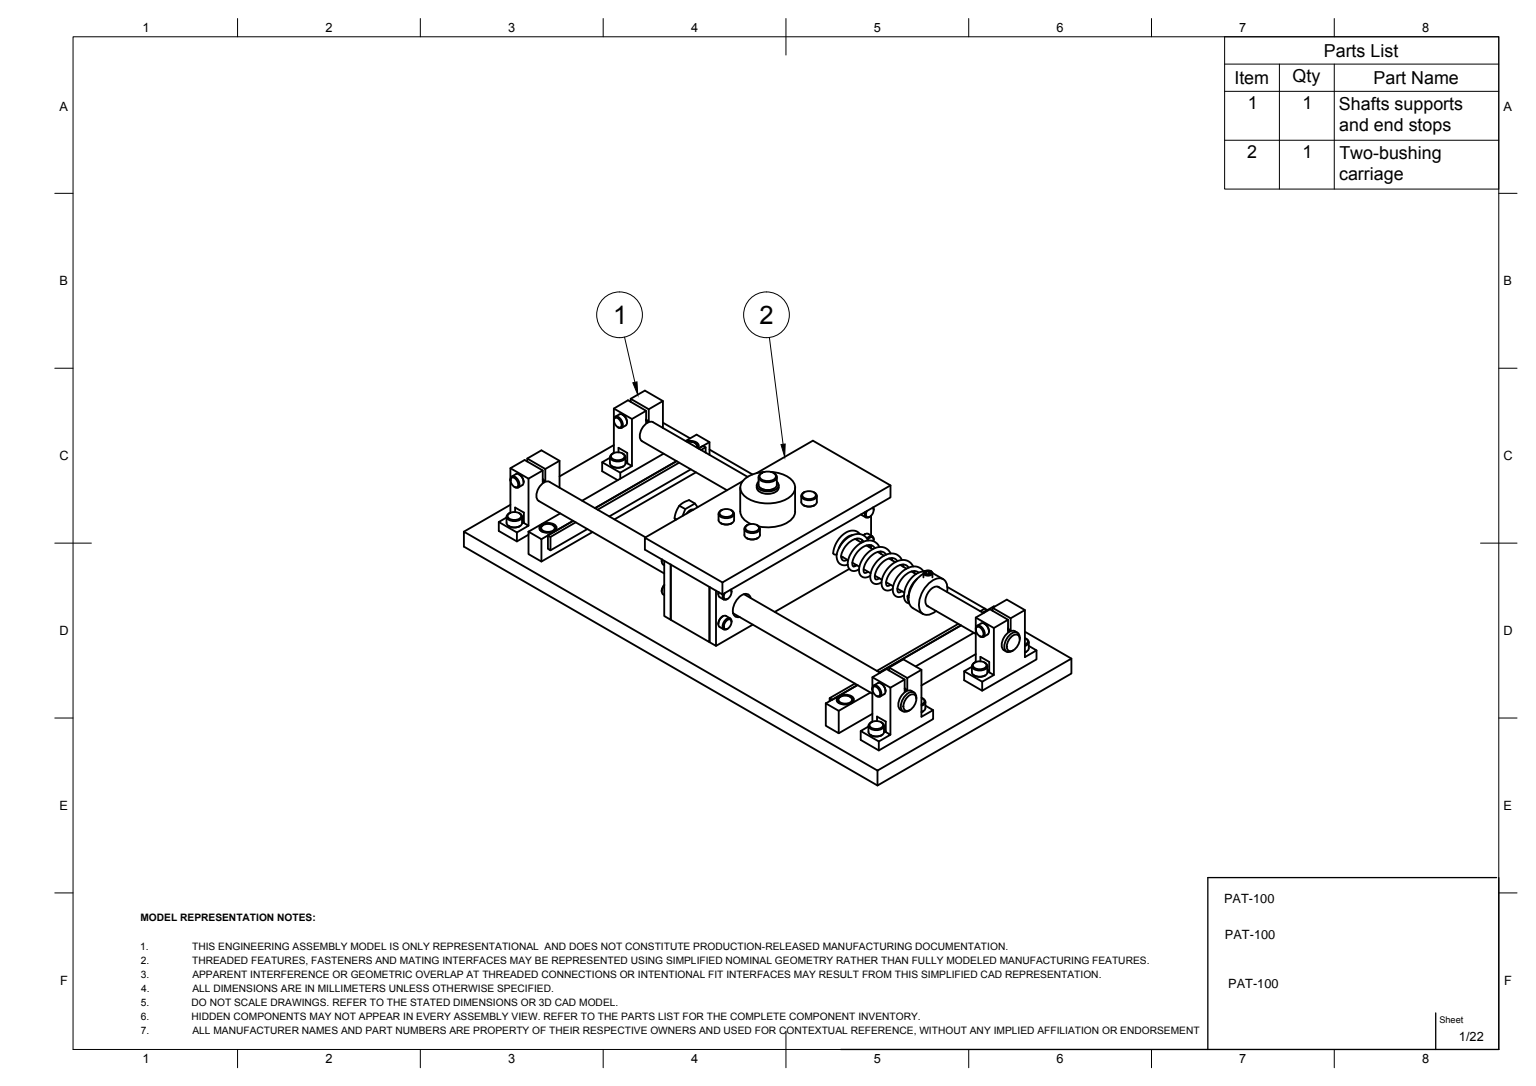
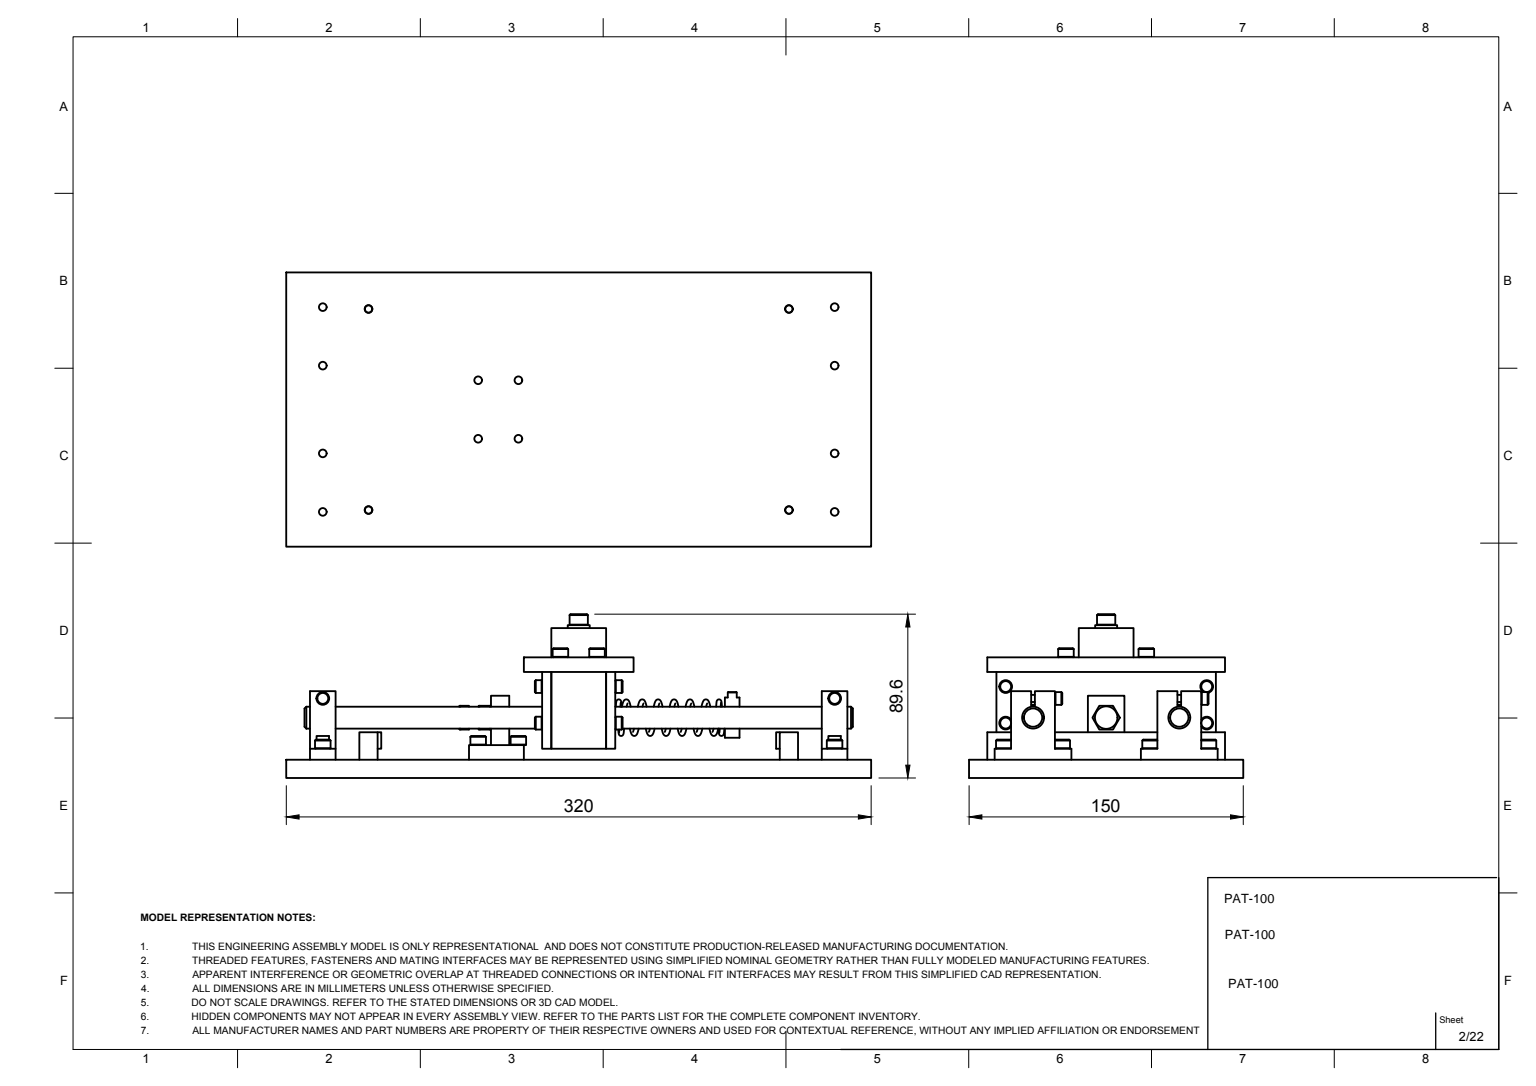
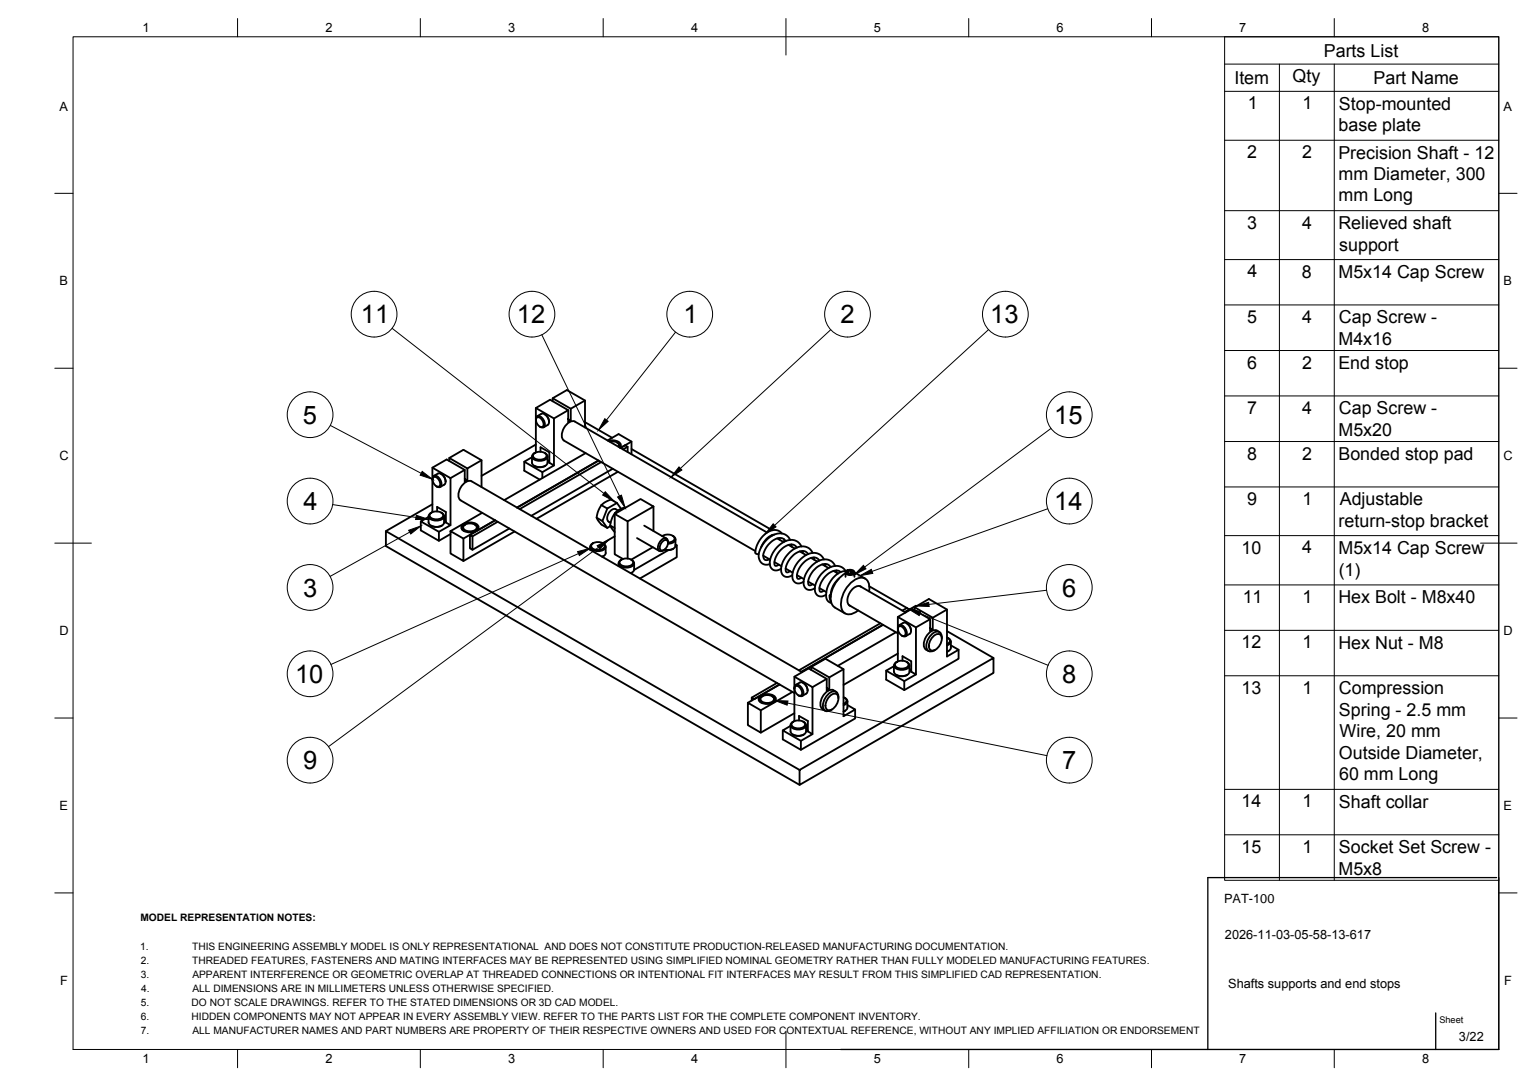
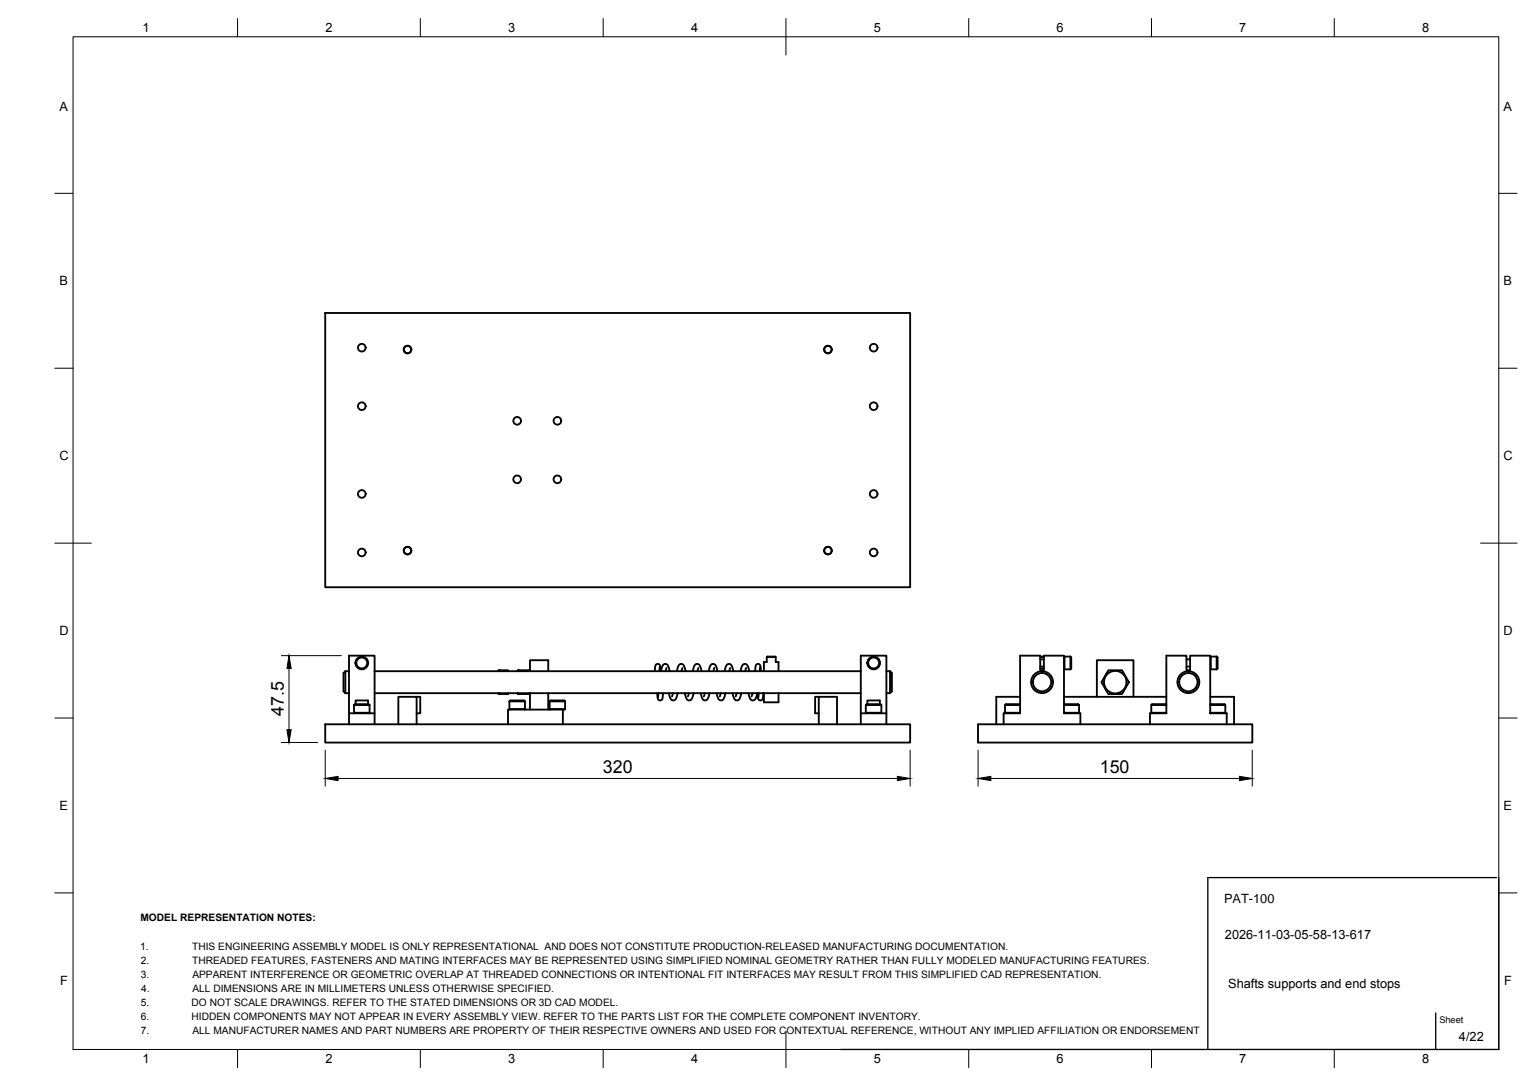
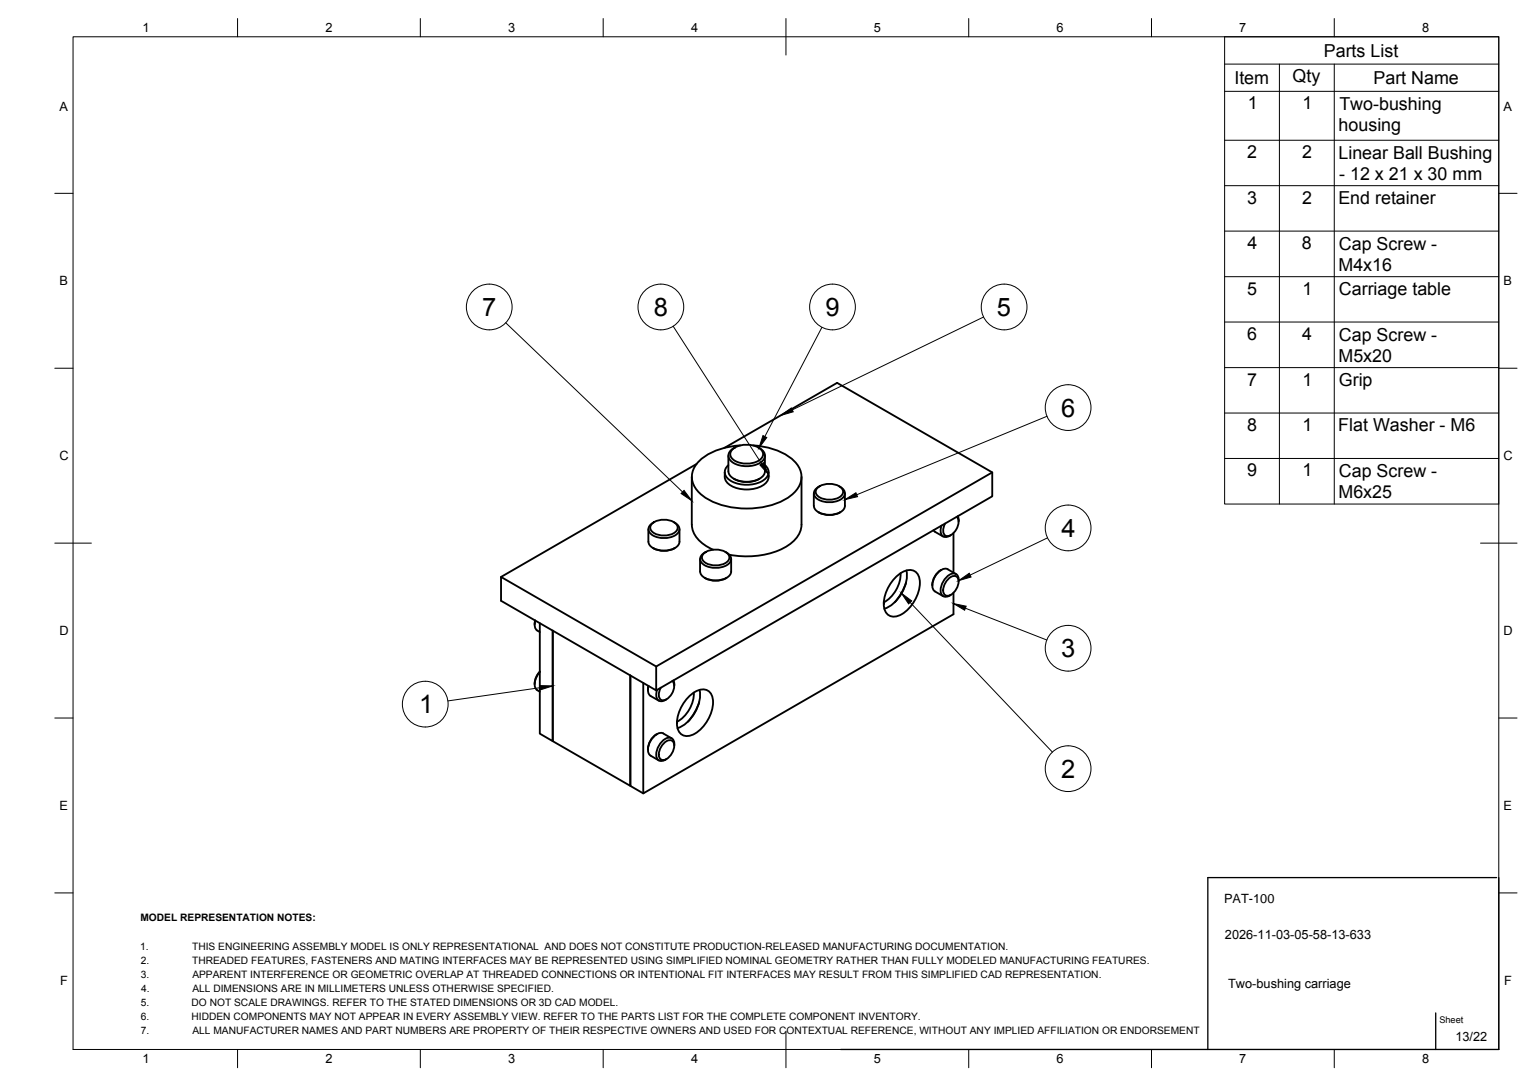
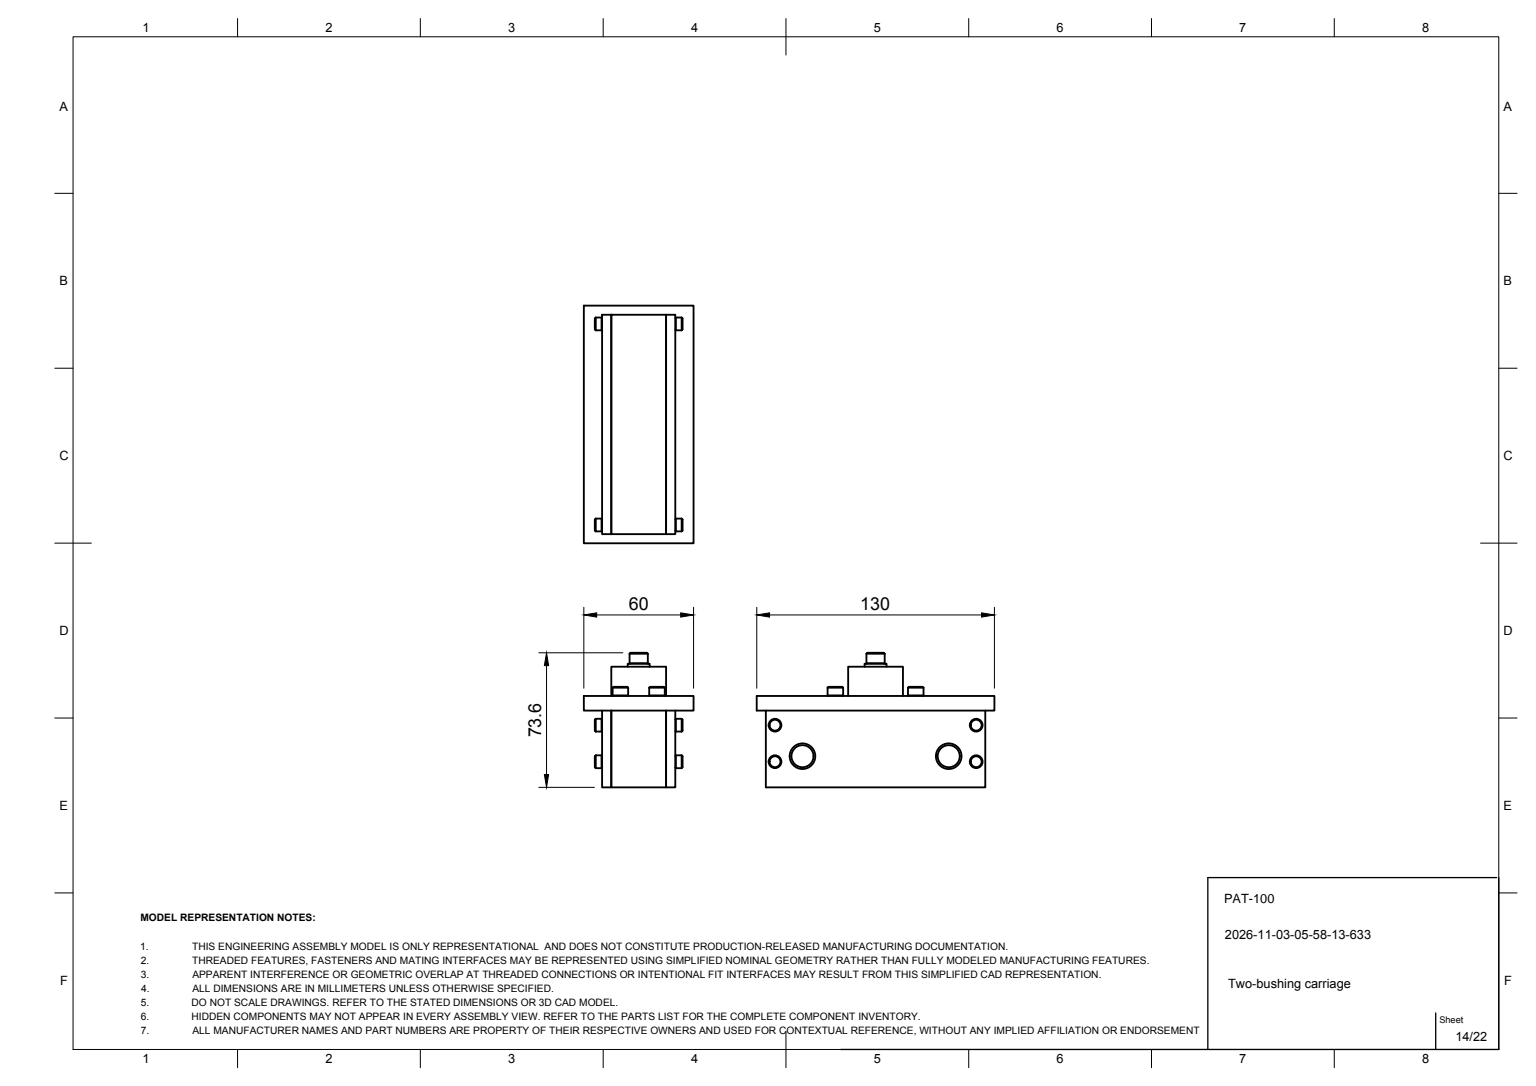
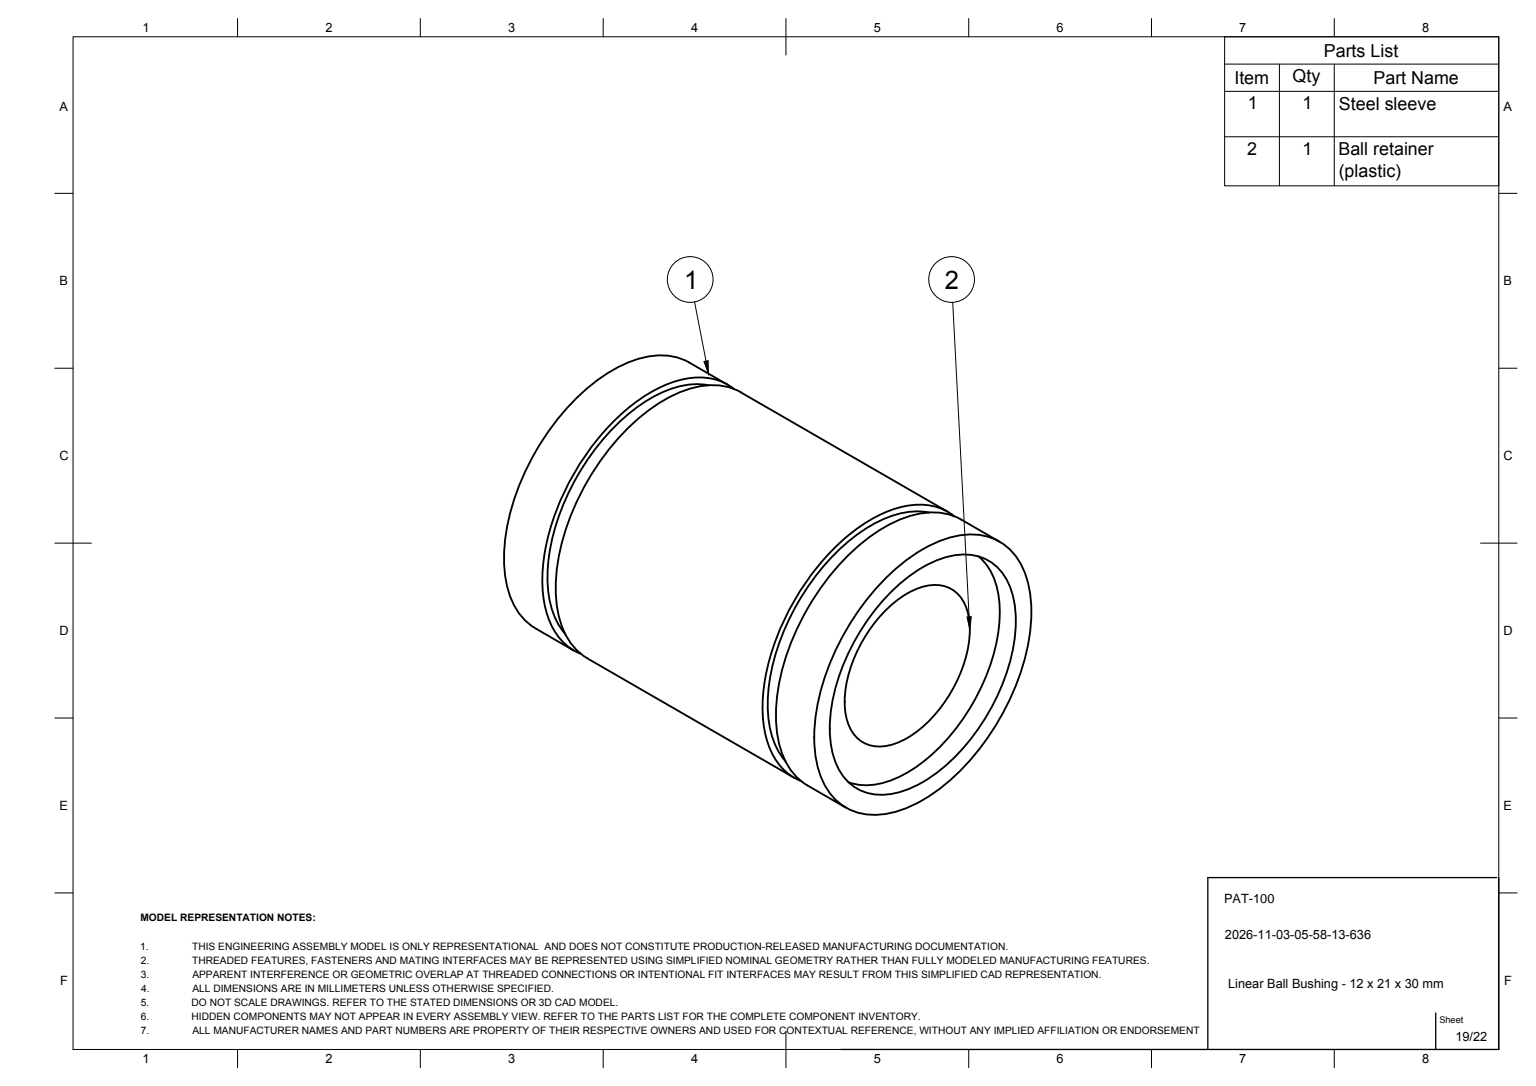
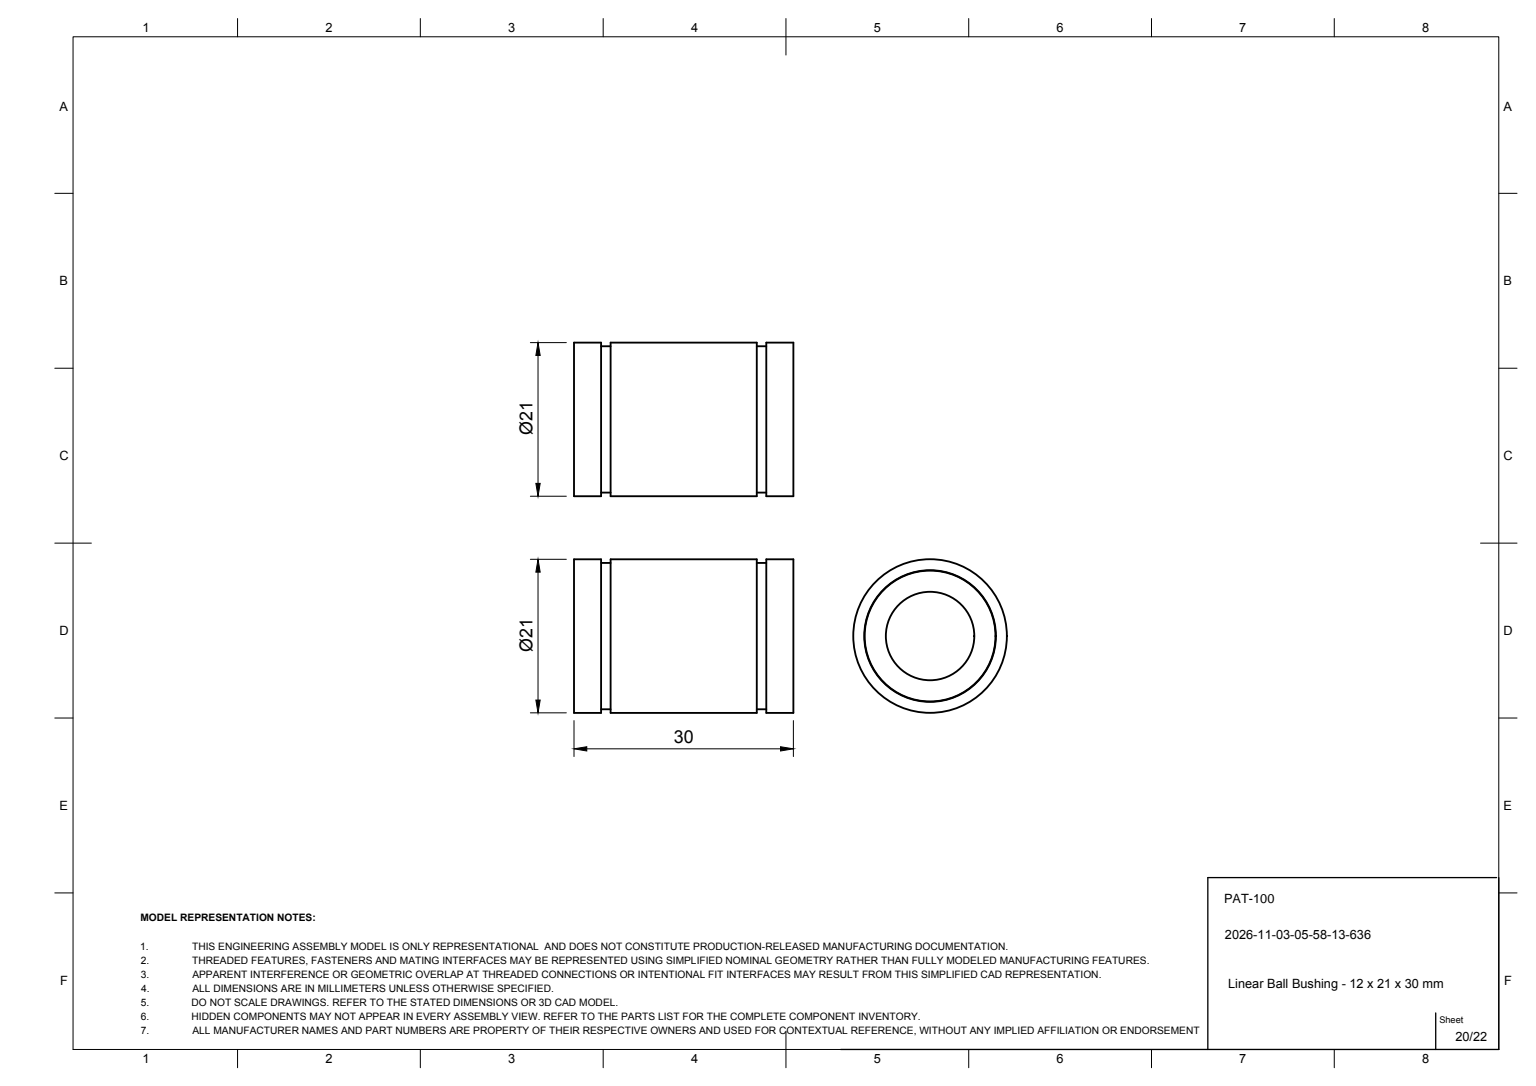
ISO-10303-21;
HEADER;
/* Generated by software containing ST-Developer
 * from STEP Tools, Inc. (www.steptools.com) 
 */

FILE_DESCRIPTION(
/* description */ (''),
/* implementation_level */ '2;1');

FILE_NAME(
/* name */ 'PAT-100',
/* time_stamp */ '2026-10-29T16:43:51-07:00',
/* author */ (''),
/* organization */ (''),
/* preprocessor_version */ 'ST-DEVELOPER v20.2',
/* originating_system */ 'Autodesk Translation Framework v15.17.0.0',
/* authorisation */ '');

FILE_SCHEMA (('AUTOMOTIVE_DESIGN { 1 0 10303 214 3 1 1 }'));
ENDSEC;

DATA;
#10=MECHANICAL_DESIGN_GEOMETRIC_PRESENTATION_REPRESENTATION('',(#365,#366,
#367,#368,#369,#370,#371,#372,#373,#374,#375,#376,#377,#378,#379,#380,#381,
#382,#383,#384,#385,#386,#387),#10292);
#11=ITEM_DEFINED_TRANSFORMATION($,$,#5632,#5681);
#12=ITEM_DEFINED_TRANSFORMATION($,$,#5664,#5682);
#13=ITEM_DEFINED_TRANSFORMATION($,$,#5291,#5760);
#14=ITEM_DEFINED_TRANSFORMATION($,$,#5346,#5761);
#15=ITEM_DEFINED_TRANSFORMATION($,$,#5356,#5762);
#16=ITEM_DEFINED_TRANSFORMATION($,$,#5394,#5763);
#17=ITEM_DEFINED_TRANSFORMATION($,$,#5394,#5764);
#18=ITEM_DEFINED_TRANSFORMATION($,$,#5708,#5765);
#19=ITEM_DEFINED_TRANSFORMATION($,$,#5356,#5766);
#20=ITEM_DEFINED_TRANSFORMATION($,$,#5394,#5767);
#21=ITEM_DEFINED_TRANSFORMATION($,$,#5394,#5768);
#22=ITEM_DEFINED_TRANSFORMATION($,$,#5708,#5769);
#23=ITEM_DEFINED_TRANSFORMATION($,$,#5346,#5770);
#24=ITEM_DEFINED_TRANSFORMATION($,$,#5356,#5771);
#25=ITEM_DEFINED_TRANSFORMATION($,$,#5394,#5772);
#26=ITEM_DEFINED_TRANSFORMATION($,$,#5394,#5773);
#27=ITEM_DEFINED_TRANSFORMATION($,$,#5708,#5774);
#28=ITEM_DEFINED_TRANSFORMATION($,$,#5356,#5775);
#29=ITEM_DEFINED_TRANSFORMATION($,$,#5394,#5776);
#30=ITEM_DEFINED_TRANSFORMATION($,$,#5394,#5777);
#31=ITEM_DEFINED_TRANSFORMATION($,$,#5708,#5778);
#32=ITEM_DEFINED_TRANSFORMATION($,$,#5418,#5779);
#33=ITEM_DEFINED_TRANSFORMATION($,$,#5734,#5780);
#34=ITEM_DEFINED_TRANSFORMATION($,$,#5734,#5781);
#35=ITEM_DEFINED_TRANSFORMATION($,$,#5418,#5782);
#36=ITEM_DEFINED_TRANSFORMATION($,$,#5734,#5783);
#37=ITEM_DEFINED_TRANSFORMATION($,$,#5734,#5784);
#38=ITEM_DEFINED_TRANSFORMATION($,$,#5439,#5785);
#39=ITEM_DEFINED_TRANSFORMATION($,$,#5439,#5786);
#40=ITEM_DEFINED_TRANSFORMATION($,$,#5446,#5787);
#41=ITEM_DEFINED_TRANSFORMATION($,$,#5473,#5788);
#42=ITEM_DEFINED_TRANSFORMATION($,$,#5473,#5789);
#43=ITEM_DEFINED_TRANSFORMATION($,$,#5473,#5790);
#44=ITEM_DEFINED_TRANSFORMATION($,$,#5473,#5791);
#45=ITEM_DEFINED_TRANSFORMATION($,$,#5497,#5792);
#46=ITEM_DEFINED_TRANSFORMATION($,$,#5514,#5793);
#47=ITEM_DEFINED_TRANSFORMATION($,$,#5530,#5794);
#48=ITEM_DEFINED_TRANSFORMATION($,$,#5535,#5795);
#49=ITEM_DEFINED_TRANSFORMATION($,$,#5550,#5796);
#50=ITEM_DEFINED_TRANSFORMATION($,$,#5568,#5841);
#51=ITEM_DEFINED_TRANSFORMATION($,$,#5609,#5842);
#52=ITEM_DEFINED_TRANSFORMATION($,$,#5631,#5843);
#53=ITEM_DEFINED_TRANSFORMATION($,$,#5631,#5844);
#54=ITEM_DEFINED_TRANSFORMATION($,$,#5683,#5845);
#55=ITEM_DEFINED_TRANSFORMATION($,$,#5683,#5846);
#56=ITEM_DEFINED_TRANSFORMATION($,$,#5708,#5847);
#57=ITEM_DEFINED_TRANSFORMATION($,$,#5708,#5848);
#58=ITEM_DEFINED_TRANSFORMATION($,$,#5708,#5849);
#59=ITEM_DEFINED_TRANSFORMATION($,$,#5708,#5850);
#60=ITEM_DEFINED_TRANSFORMATION($,$,#5708,#5851);
#61=ITEM_DEFINED_TRANSFORMATION($,$,#5708,#5852);
#62=ITEM_DEFINED_TRANSFORMATION($,$,#5708,#5853);
#63=ITEM_DEFINED_TRANSFORMATION($,$,#5708,#5854);
#64=ITEM_DEFINED_TRANSFORMATION($,$,#5734,#5855);
#65=ITEM_DEFINED_TRANSFORMATION($,$,#5734,#5856);
#66=ITEM_DEFINED_TRANSFORMATION($,$,#5734,#5857);
#67=ITEM_DEFINED_TRANSFORMATION($,$,#5734,#5858);
#68=ITEM_DEFINED_TRANSFORMATION($,$,#5797,#5859);
#69=ITEM_DEFINED_TRANSFORMATION($,$,#5806,#5860);
#70=ITEM_DEFINED_TRANSFORMATION($,$,#5815,#5861);
#71=ITEM_DEFINED_TRANSFORMATION($,$,#5290,#5862);
#72=ITEM_DEFINED_TRANSFORMATION($,$,#5567,#5863);
#73=(
REPRESENTATION_RELATIONSHIP($,$,#10432,#10431)
REPRESENTATION_RELATIONSHIP_WITH_TRANSFORMATION(#11)
SHAPE_REPRESENTATION_RELATIONSHIP()
);
#74=(
REPRESENTATION_RELATIONSHIP($,$,#10433,#10431)
REPRESENTATION_RELATIONSHIP_WITH_TRANSFORMATION(#12)
SHAPE_REPRESENTATION_RELATIONSHIP()
);
#75=(
REPRESENTATION_RELATIONSHIP($,$,#10415,#10414)
REPRESENTATION_RELATIONSHIP_WITH_TRANSFORMATION(#13)
SHAPE_REPRESENTATION_RELATIONSHIP()
);
#76=(
REPRESENTATION_RELATIONSHIP($,$,#10416,#10414)
REPRESENTATION_RELATIONSHIP_WITH_TRANSFORMATION(#14)
SHAPE_REPRESENTATION_RELATIONSHIP()
);
#77=(
REPRESENTATION_RELATIONSHIP($,$,#10417,#10414)
REPRESENTATION_RELATIONSHIP_WITH_TRANSFORMATION(#15)
SHAPE_REPRESENTATION_RELATIONSHIP()
);
#78=(
REPRESENTATION_RELATIONSHIP($,$,#10418,#10414)
REPRESENTATION_RELATIONSHIP_WITH_TRANSFORMATION(#16)
SHAPE_REPRESENTATION_RELATIONSHIP()
);
#79=(
REPRESENTATION_RELATIONSHIP($,$,#10418,#10414)
REPRESENTATION_RELATIONSHIP_WITH_TRANSFORMATION(#17)
SHAPE_REPRESENTATION_RELATIONSHIP()
);
#80=(
REPRESENTATION_RELATIONSHIP($,$,#10435,#10414)
REPRESENTATION_RELATIONSHIP_WITH_TRANSFORMATION(#18)
SHAPE_REPRESENTATION_RELATIONSHIP()
);
#81=(
REPRESENTATION_RELATIONSHIP($,$,#10417,#10414)
REPRESENTATION_RELATIONSHIP_WITH_TRANSFORMATION(#19)
SHAPE_REPRESENTATION_RELATIONSHIP()
);
#82=(
REPRESENTATION_RELATIONSHIP($,$,#10418,#10414)
REPRESENTATION_RELATIONSHIP_WITH_TRANSFORMATION(#20)
SHAPE_REPRESENTATION_RELATIONSHIP()
);
#83=(
REPRESENTATION_RELATIONSHIP($,$,#10418,#10414)
REPRESENTATION_RELATIONSHIP_WITH_TRANSFORMATION(#21)
SHAPE_REPRESENTATION_RELATIONSHIP()
);
#84=(
REPRESENTATION_RELATIONSHIP($,$,#10435,#10414)
REPRESENTATION_RELATIONSHIP_WITH_TRANSFORMATION(#22)
SHAPE_REPRESENTATION_RELATIONSHIP()
);
#85=(
REPRESENTATION_RELATIONSHIP($,$,#10416,#10414)
REPRESENTATION_RELATIONSHIP_WITH_TRANSFORMATION(#23)
SHAPE_REPRESENTATION_RELATIONSHIP()
);
#86=(
REPRESENTATION_RELATIONSHIP($,$,#10417,#10414)
REPRESENTATION_RELATIONSHIP_WITH_TRANSFORMATION(#24)
SHAPE_REPRESENTATION_RELATIONSHIP()
);
#87=(
REPRESENTATION_RELATIONSHIP($,$,#10418,#10414)
REPRESENTATION_RELATIONSHIP_WITH_TRANSFORMATION(#25)
SHAPE_REPRESENTATION_RELATIONSHIP()
);
#88=(
REPRESENTATION_RELATIONSHIP($,$,#10418,#10414)
REPRESENTATION_RELATIONSHIP_WITH_TRANSFORMATION(#26)
SHAPE_REPRESENTATION_RELATIONSHIP()
);
#89=(
REPRESENTATION_RELATIONSHIP($,$,#10435,#10414)
REPRESENTATION_RELATIONSHIP_WITH_TRANSFORMATION(#27)
SHAPE_REPRESENTATION_RELATIONSHIP()
);
#90=(
REPRESENTATION_RELATIONSHIP($,$,#10417,#10414)
REPRESENTATION_RELATIONSHIP_WITH_TRANSFORMATION(#28)
SHAPE_REPRESENTATION_RELATIONSHIP()
);
#91=(
REPRESENTATION_RELATIONSHIP($,$,#10418,#10414)
REPRESENTATION_RELATIONSHIP_WITH_TRANSFORMATION(#29)
SHAPE_REPRESENTATION_RELATIONSHIP()
);
#92=(
REPRESENTATION_RELATIONSHIP($,$,#10418,#10414)
REPRESENTATION_RELATIONSHIP_WITH_TRANSFORMATION(#30)
SHAPE_REPRESENTATION_RELATIONSHIP()
);
#93=(
REPRESENTATION_RELATIONSHIP($,$,#10435,#10414)
REPRESENTATION_RELATIONSHIP_WITH_TRANSFORMATION(#31)
SHAPE_REPRESENTATION_RELATIONSHIP()
);
#94=(
REPRESENTATION_RELATIONSHIP($,$,#10419,#10414)
REPRESENTATION_RELATIONSHIP_WITH_TRANSFORMATION(#32)
SHAPE_REPRESENTATION_RELATIONSHIP()
);
#95=(
REPRESENTATION_RELATIONSHIP($,$,#10436,#10414)
REPRESENTATION_RELATIONSHIP_WITH_TRANSFORMATION(#33)
SHAPE_REPRESENTATION_RELATIONSHIP()
);
#96=(
REPRESENTATION_RELATIONSHIP($,$,#10436,#10414)
REPRESENTATION_RELATIONSHIP_WITH_TRANSFORMATION(#34)
SHAPE_REPRESENTATION_RELATIONSHIP()
);
#97=(
REPRESENTATION_RELATIONSHIP($,$,#10419,#10414)
REPRESENTATION_RELATIONSHIP_WITH_TRANSFORMATION(#35)
SHAPE_REPRESENTATION_RELATIONSHIP()
);
#98=(
REPRESENTATION_RELATIONSHIP($,$,#10436,#10414)
REPRESENTATION_RELATIONSHIP_WITH_TRANSFORMATION(#36)
SHAPE_REPRESENTATION_RELATIONSHIP()
);
#99=(
REPRESENTATION_RELATIONSHIP($,$,#10436,#10414)
REPRESENTATION_RELATIONSHIP_WITH_TRANSFORMATION(#37)
SHAPE_REPRESENTATION_RELATIONSHIP()
);
#100=(
REPRESENTATION_RELATIONSHIP($,$,#10420,#10414)
REPRESENTATION_RELATIONSHIP_WITH_TRANSFORMATION(#38)
SHAPE_REPRESENTATION_RELATIONSHIP()
);
#101=(
REPRESENTATION_RELATIONSHIP($,$,#10420,#10414)
REPRESENTATION_RELATIONSHIP_WITH_TRANSFORMATION(#39)
SHAPE_REPRESENTATION_RELATIONSHIP()
);
#102=(
REPRESENTATION_RELATIONSHIP($,$,#10421,#10414)
REPRESENTATION_RELATIONSHIP_WITH_TRANSFORMATION(#40)
SHAPE_REPRESENTATION_RELATIONSHIP()
);
#103=(
REPRESENTATION_RELATIONSHIP($,$,#10422,#10414)
REPRESENTATION_RELATIONSHIP_WITH_TRANSFORMATION(#41)
SHAPE_REPRESENTATION_RELATIONSHIP()
);
#104=(
REPRESENTATION_RELATIONSHIP($,$,#10422,#10414)
REPRESENTATION_RELATIONSHIP_WITH_TRANSFORMATION(#42)
SHAPE_REPRESENTATION_RELATIONSHIP()
);
#105=(
REPRESENTATION_RELATIONSHIP($,$,#10422,#10414)
REPRESENTATION_RELATIONSHIP_WITH_TRANSFORMATION(#43)
SHAPE_REPRESENTATION_RELATIONSHIP()
);
#106=(
REPRESENTATION_RELATIONSHIP($,$,#10422,#10414)
REPRESENTATION_RELATIONSHIP_WITH_TRANSFORMATION(#44)
SHAPE_REPRESENTATION_RELATIONSHIP()
);
#107=(
REPRESENTATION_RELATIONSHIP($,$,#10423,#10414)
REPRESENTATION_RELATIONSHIP_WITH_TRANSFORMATION(#45)
SHAPE_REPRESENTATION_RELATIONSHIP()
);
#108=(
REPRESENTATION_RELATIONSHIP($,$,#10424,#10414)
REPRESENTATION_RELATIONSHIP_WITH_TRANSFORMATION(#46)
SHAPE_REPRESENTATION_RELATIONSHIP()
);
#109=(
REPRESENTATION_RELATIONSHIP($,$,#10425,#10414)
REPRESENTATION_RELATIONSHIP_WITH_TRANSFORMATION(#47)
SHAPE_REPRESENTATION_RELATIONSHIP()
);
#110=(
REPRESENTATION_RELATIONSHIP($,$,#10426,#10414)
REPRESENTATION_RELATIONSHIP_WITH_TRANSFORMATION(#48)
SHAPE_REPRESENTATION_RELATIONSHIP()
);
#111=(
REPRESENTATION_RELATIONSHIP($,$,#10427,#10414)
REPRESENTATION_RELATIONSHIP_WITH_TRANSFORMATION(#49)
SHAPE_REPRESENTATION_RELATIONSHIP()
);
#112=(
REPRESENTATION_RELATIONSHIP($,$,#10429,#10428)
REPRESENTATION_RELATIONSHIP_WITH_TRANSFORMATION(#50)
SHAPE_REPRESENTATION_RELATIONSHIP()
);
#113=(
REPRESENTATION_RELATIONSHIP($,$,#10430,#10428)
REPRESENTATION_RELATIONSHIP_WITH_TRANSFORMATION(#51)
SHAPE_REPRESENTATION_RELATIONSHIP()
);
#114=(
REPRESENTATION_RELATIONSHIP($,$,#10431,#10428)
REPRESENTATION_RELATIONSHIP_WITH_TRANSFORMATION(#52)
SHAPE_REPRESENTATION_RELATIONSHIP()
);
#115=(
REPRESENTATION_RELATIONSHIP($,$,#10431,#10428)
REPRESENTATION_RELATIONSHIP_WITH_TRANSFORMATION(#53)
SHAPE_REPRESENTATION_RELATIONSHIP()
);
#116=(
REPRESENTATION_RELATIONSHIP($,$,#10434,#10428)
REPRESENTATION_RELATIONSHIP_WITH_TRANSFORMATION(#54)
SHAPE_REPRESENTATION_RELATIONSHIP()
);
#117=(
REPRESENTATION_RELATIONSHIP($,$,#10434,#10428)
REPRESENTATION_RELATIONSHIP_WITH_TRANSFORMATION(#55)
SHAPE_REPRESENTATION_RELATIONSHIP()
);
#118=(
REPRESENTATION_RELATIONSHIP($,$,#10435,#10428)
REPRESENTATION_RELATIONSHIP_WITH_TRANSFORMATION(#56)
SHAPE_REPRESENTATION_RELATIONSHIP()
);
#119=(
REPRESENTATION_RELATIONSHIP($,$,#10435,#10428)
REPRESENTATION_RELATIONSHIP_WITH_TRANSFORMATION(#57)
SHAPE_REPRESENTATION_RELATIONSHIP()
);
#120=(
REPRESENTATION_RELATIONSHIP($,$,#10435,#10428)
REPRESENTATION_RELATIONSHIP_WITH_TRANSFORMATION(#58)
SHAPE_REPRESENTATION_RELATIONSHIP()
);
#121=(
REPRESENTATION_RELATIONSHIP($,$,#10435,#10428)
REPRESENTATION_RELATIONSHIP_WITH_TRANSFORMATION(#59)
SHAPE_REPRESENTATION_RELATIONSHIP()
);
#122=(
REPRESENTATION_RELATIONSHIP($,$,#10435,#10428)
REPRESENTATION_RELATIONSHIP_WITH_TRANSFORMATION(#60)
SHAPE_REPRESENTATION_RELATIONSHIP()
);
#123=(
REPRESENTATION_RELATIONSHIP($,$,#10435,#10428)
REPRESENTATION_RELATIONSHIP_WITH_TRANSFORMATION(#61)
SHAPE_REPRESENTATION_RELATIONSHIP()
);
#124=(
REPRESENTATION_RELATIONSHIP($,$,#10435,#10428)
REPRESENTATION_RELATIONSHIP_WITH_TRANSFORMATION(#62)
SHAPE_REPRESENTATION_RELATIONSHIP()
);
#125=(
REPRESENTATION_RELATIONSHIP($,$,#10435,#10428)
REPRESENTATION_RELATIONSHIP_WITH_TRANSFORMATION(#63)
SHAPE_REPRESENTATION_RELATIONSHIP()
);
#126=(
REPRESENTATION_RELATIONSHIP($,$,#10436,#10428)
REPRESENTATION_RELATIONSHIP_WITH_TRANSFORMATION(#64)
SHAPE_REPRESENTATION_RELATIONSHIP()
);
#127=(
REPRESENTATION_RELATIONSHIP($,$,#10436,#10428)
REPRESENTATION_RELATIONSHIP_WITH_TRANSFORMATION(#65)
SHAPE_REPRESENTATION_RELATIONSHIP()
);
#128=(
REPRESENTATION_RELATIONSHIP($,$,#10436,#10428)
REPRESENTATION_RELATIONSHIP_WITH_TRANSFORMATION(#66)
SHAPE_REPRESENTATION_RELATIONSHIP()
);
#129=(
REPRESENTATION_RELATIONSHIP($,$,#10436,#10428)
REPRESENTATION_RELATIONSHIP_WITH_TRANSFORMATION(#67)
SHAPE_REPRESENTATION_RELATIONSHIP()
);
#130=(
REPRESENTATION_RELATIONSHIP($,$,#10437,#10428)
REPRESENTATION_RELATIONSHIP_WITH_TRANSFORMATION(#68)
SHAPE_REPRESENTATION_RELATIONSHIP()
);
#131=(
REPRESENTATION_RELATIONSHIP($,$,#10438,#10428)
REPRESENTATION_RELATIONSHIP_WITH_TRANSFORMATION(#69)
SHAPE_REPRESENTATION_RELATIONSHIP()
);
#132=(
REPRESENTATION_RELATIONSHIP($,$,#10439,#10428)
REPRESENTATION_RELATIONSHIP_WITH_TRANSFORMATION(#70)
SHAPE_REPRESENTATION_RELATIONSHIP()
);
#133=(
REPRESENTATION_RELATIONSHIP($,$,#10414,#10413)
REPRESENTATION_RELATIONSHIP_WITH_TRANSFORMATION(#71)
SHAPE_REPRESENTATION_RELATIONSHIP()
);
#134=(
REPRESENTATION_RELATIONSHIP($,$,#10428,#10413)
REPRESENTATION_RELATIONSHIP_WITH_TRANSFORMATION(#72)
SHAPE_REPRESENTATION_RELATIONSHIP()
);
#135=CONTEXT_DEPENDENT_SHAPE_REPRESENTATION(#73,#10345);
#136=CONTEXT_DEPENDENT_SHAPE_REPRESENTATION(#74,#10346);
#137=CONTEXT_DEPENDENT_SHAPE_REPRESENTATION(#75,#10350);
#138=CONTEXT_DEPENDENT_SHAPE_REPRESENTATION(#76,#10351);
#139=CONTEXT_DEPENDENT_SHAPE_REPRESENTATION(#77,#10352);
#140=CONTEXT_DEPENDENT_SHAPE_REPRESENTATION(#78,#10353);
#141=CONTEXT_DEPENDENT_SHAPE_REPRESENTATION(#79,#10354);
#142=CONTEXT_DEPENDENT_SHAPE_REPRESENTATION(#80,#10355);
#143=CONTEXT_DEPENDENT_SHAPE_REPRESENTATION(#81,#10356);
#144=CONTEXT_DEPENDENT_SHAPE_REPRESENTATION(#82,#10357);
#145=CONTEXT_DEPENDENT_SHAPE_REPRESENTATION(#83,#10358);
#146=CONTEXT_DEPENDENT_SHAPE_REPRESENTATION(#84,#10359);
#147=CONTEXT_DEPENDENT_SHAPE_REPRESENTATION(#85,#10360);
#148=CONTEXT_DEPENDENT_SHAPE_REPRESENTATION(#86,#10361);
#149=CONTEXT_DEPENDENT_SHAPE_REPRESENTATION(#87,#10362);
#150=CONTEXT_DEPENDENT_SHAPE_REPRESENTATION(#88,#10363);
#151=CONTEXT_DEPENDENT_SHAPE_REPRESENTATION(#89,#10364);
#152=CONTEXT_DEPENDENT_SHAPE_REPRESENTATION(#90,#10365);
#153=CONTEXT_DEPENDENT_SHAPE_REPRESENTATION(#91,#10366);
#154=CONTEXT_DEPENDENT_SHAPE_REPRESENTATION(#92,#10367);
#155=CONTEXT_DEPENDENT_SHAPE_REPRESENTATION(#93,#10368);
#156=CONTEXT_DEPENDENT_SHAPE_REPRESENTATION(#94,#10369);
#157=CONTEXT_DEPENDENT_SHAPE_REPRESENTATION(#95,#10370);
#158=CONTEXT_DEPENDENT_SHAPE_REPRESENTATION(#96,#10371);
#159=CONTEXT_DEPENDENT_SHAPE_REPRESENTATION(#97,#10372);
#160=CONTEXT_DEPENDENT_SHAPE_REPRESENTATION(#98,#10373);
#161=CONTEXT_DEPENDENT_SHAPE_REPRESENTATION(#99,#10374);
#162=CONTEXT_DEPENDENT_SHAPE_REPRESENTATION(#100,#10375);
#163=CONTEXT_DEPENDENT_SHAPE_REPRESENTATION(#101,#10376);
#164=CONTEXT_DEPENDENT_SHAPE_REPRESENTATION(#102,#10377);
#165=CONTEXT_DEPENDENT_SHAPE_REPRESENTATION(#103,#10378);
#166=CONTEXT_DEPENDENT_SHAPE_REPRESENTATION(#104,#10379);
#167=CONTEXT_DEPENDENT_SHAPE_REPRESENTATION(#105,#10380);
#168=CONTEXT_DEPENDENT_SHAPE_REPRESENTATION(#106,#10381);
#169=CONTEXT_DEPENDENT_SHAPE_REPRESENTATION(#107,#10382);
#170=CONTEXT_DEPENDENT_SHAPE_REPRESENTATION(#108,#10383);
#171=CONTEXT_DEPENDENT_SHAPE_REPRESENTATION(#109,#10384);
#172=CONTEXT_DEPENDENT_SHAPE_REPRESENTATION(#110,#10385);
#173=CONTEXT_DEPENDENT_SHAPE_REPRESENTATION(#111,#10386);
#174=CONTEXT_DEPENDENT_SHAPE_REPRESENTATION(#112,#10390);
#175=CONTEXT_DEPENDENT_SHAPE_REPRESENTATION(#113,#10391);
#176=CONTEXT_DEPENDENT_SHAPE_REPRESENTATION(#114,#10392);
#177=CONTEXT_DEPENDENT_SHAPE_REPRESENTATION(#115,#10393);
#178=CONTEXT_DEPENDENT_SHAPE_REPRESENTATION(#116,#10394);
#179=CONTEXT_DEPENDENT_SHAPE_REPRESENTATION(#117,#10395);
#180=CONTEXT_DEPENDENT_SHAPE_REPRESENTATION(#118,#10396);
#181=CONTEXT_DEPENDENT_SHAPE_REPRESENTATION(#119,#10397);
#182=CONTEXT_DEPENDENT_SHAPE_REPRESENTATION(#120,#10398);
#183=CONTEXT_DEPENDENT_SHAPE_REPRESENTATION(#121,#10399);
#184=CONTEXT_DEPENDENT_SHAPE_REPRESENTATION(#122,#10400);
#185=CONTEXT_DEPENDENT_SHAPE_REPRESENTATION(#123,#10401);
#186=CONTEXT_DEPENDENT_SHAPE_REPRESENTATION(#124,#10402);
#187=CONTEXT_DEPENDENT_SHAPE_REPRESENTATION(#125,#10403);
#188=CONTEXT_DEPENDENT_SHAPE_REPRESENTATION(#126,#10404);
#189=CONTEXT_DEPENDENT_SHAPE_REPRESENTATION(#127,#10405);
#190=CONTEXT_DEPENDENT_SHAPE_REPRESENTATION(#128,#10406);
#191=CONTEXT_DEPENDENT_SHAPE_REPRESENTATION(#129,#10407);
#192=CONTEXT_DEPENDENT_SHAPE_REPRESENTATION(#130,#10408);
#193=CONTEXT_DEPENDENT_SHAPE_REPRESENTATION(#131,#10409);
#194=CONTEXT_DEPENDENT_SHAPE_REPRESENTATION(#132,#10410);
#195=CONTEXT_DEPENDENT_SHAPE_REPRESENTATION(#133,#10411);
#196=CONTEXT_DEPENDENT_SHAPE_REPRESENTATION(#134,#10412);
#197=NEXT_ASSEMBLY_USAGE_OCCURRENCE('Steel sleeve:1','Steel sleeve:1',
'Steel sleeve:1',#10459,#10460,'Steel sleeve:1');
#198=NEXT_ASSEMBLY_USAGE_OCCURRENCE('Ball retainer (plastic):1',
'Ball retainer (plastic):1','Ball retainer (plastic):1',#10459,#10461,
'Ball retainer (plastic):1');
#199=NEXT_ASSEMBLY_USAGE_OCCURRENCE('Stop-mounted base plate:2',
'Stop-mounted base plate:2','Stop-mounted base plate:2',#10442,#10443,
'Stop-mounted base plate:2');
#200=NEXT_ASSEMBLY_USAGE_OCCURRENCE(
'Precision Shaft - 12 mm Diameter, 300 mm Long:2',
'Precision Shaft - 12 mm Diameter, 300 mm Long:2',
'Precision Shaft - 12 mm Diameter, 300 mm Long:2',#10442,#10444,
'Precision Shaft - 12 mm Diameter, 300 mm Long:2');
#201=NEXT_ASSEMBLY_USAGE_OCCURRENCE('Relieved shaft support:2',
'Relieved shaft support:2','Relieved shaft support:2',#10442,#10445,
'Relieved shaft support:2');
#202=NEXT_ASSEMBLY_USAGE_OCCURRENCE('M5x14 Cap Screw:2',
'M5x14 Cap Screw:2','M5x14 Cap Screw:2',#10442,#10446,
'M5x14 Cap Screw:2');
#203=NEXT_ASSEMBLY_USAGE_OCCURRENCE('M5x14 Cap Screw:3',
'M5x14 Cap Screw:3','M5x14 Cap Screw:3',#10442,#10446,
'M5x14 Cap Screw:3');
#204=NEXT_ASSEMBLY_USAGE_OCCURRENCE('Cap Screw - M4x16:2',
'Cap Screw - M4x16:2','Cap Screw - M4x16:2',#10442,#10463,
'Cap Screw - M4x16:2');
#205=NEXT_ASSEMBLY_USAGE_OCCURRENCE('Relieved shaft support:3',
'Relieved shaft support:3','Relieved shaft support:3',#10442,#10445,
'Relieved shaft support:3');
#206=NEXT_ASSEMBLY_USAGE_OCCURRENCE('M5x14 Cap Screw:4',
'M5x14 Cap Screw:4','M5x14 Cap Screw:4',#10442,#10446,
'M5x14 Cap Screw:4');
#207=NEXT_ASSEMBLY_USAGE_OCCURRENCE('M5x14 Cap Screw:5',
'M5x14 Cap Screw:5','M5x14 Cap Screw:5',#10442,#10446,
'M5x14 Cap Screw:5');
#208=NEXT_ASSEMBLY_USAGE_OCCURRENCE('Cap Screw - M4x16:3',
'Cap Screw - M4x16:3','Cap Screw - M4x16:3',#10442,#10463,
'Cap Screw - M4x16:3');
#209=NEXT_ASSEMBLY_USAGE_OCCURRENCE(
'Precision Shaft - 12 mm Diameter, 300 mm Long:3',
'Precision Shaft - 12 mm Diameter, 300 mm Long:3',
'Precision Shaft - 12 mm Diameter, 300 mm Long:3',#10442,#10444,
'Precision Shaft - 12 mm Diameter, 300 mm Long:3');
#210=NEXT_ASSEMBLY_USAGE_OCCURRENCE('Relieved shaft support:4',
'Relieved shaft support:4','Relieved shaft support:4',#10442,#10445,
'Relieved shaft support:4');
#211=NEXT_ASSEMBLY_USAGE_OCCURRENCE('M5x14 Cap Screw:6',
'M5x14 Cap Screw:6','M5x14 Cap Screw:6',#10442,#10446,
'M5x14 Cap Screw:6');
#212=NEXT_ASSEMBLY_USAGE_OCCURRENCE('M5x14 Cap Screw:7',
'M5x14 Cap Screw:7','M5x14 Cap Screw:7',#10442,#10446,
'M5x14 Cap Screw:7');
#213=NEXT_ASSEMBLY_USAGE_OCCURRENCE('Cap Screw - M4x16:4',
'Cap Screw - M4x16:4','Cap Screw - M4x16:4',#10442,#10463,
'Cap Screw - M4x16:4');
#214=NEXT_ASSEMBLY_USAGE_OCCURRENCE('Relieved shaft support:5',
'Relieved shaft support:5','Relieved shaft support:5',#10442,#10445,
'Relieved shaft support:5');
#215=NEXT_ASSEMBLY_USAGE_OCCURRENCE('M5x14 Cap Screw:8',
'M5x14 Cap Screw:8','M5x14 Cap Screw:8',#10442,#10446,
'M5x14 Cap Screw:8');
#216=NEXT_ASSEMBLY_USAGE_OCCURRENCE('M5x14 Cap Screw:9',
'M5x14 Cap Screw:9','M5x14 Cap Screw:9',#10442,#10446,
'M5x14 Cap Screw:9');
#217=NEXT_ASSEMBLY_USAGE_OCCURRENCE('Cap Screw - M4x16:5',
'Cap Screw - M4x16:5','Cap Screw - M4x16:5',#10442,#10463,
'Cap Screw - M4x16:5');
#218=NEXT_ASSEMBLY_USAGE_OCCURRENCE('End stop:2','End stop:2',
'End stop:2',#10442,#10447,'End stop:2');
#219=NEXT_ASSEMBLY_USAGE_OCCURRENCE('Cap Screw - M5x20:6',
'Cap Screw - M5x20:6','Cap Screw - M5x20:6',#10442,#10464,
'Cap Screw - M5x20:6');
#220=NEXT_ASSEMBLY_USAGE_OCCURRENCE('Cap Screw - M5x20:7',
'Cap Screw - M5x20:7','Cap Screw - M5x20:7',#10442,#10464,
'Cap Screw - M5x20:7');
#221=NEXT_ASSEMBLY_USAGE_OCCURRENCE('End stop:3','End stop:3',
'End stop:3',#10442,#10447,'End stop:3');
#222=NEXT_ASSEMBLY_USAGE_OCCURRENCE('Cap Screw - M5x20:8',
'Cap Screw - M5x20:8','Cap Screw - M5x20:8',#10442,#10464,
'Cap Screw - M5x20:8');
#223=NEXT_ASSEMBLY_USAGE_OCCURRENCE('Cap Screw - M5x20:9',
'Cap Screw - M5x20:9','Cap Screw - M5x20:9',#10442,#10464,
'Cap Screw - M5x20:9');
#224=NEXT_ASSEMBLY_USAGE_OCCURRENCE('Bonded stop pad:2',
'Bonded stop pad:2','Bonded stop pad:2',#10442,#10448,
'Bonded stop pad:2');
#225=NEXT_ASSEMBLY_USAGE_OCCURRENCE('Bonded stop pad:3',
'Bonded stop pad:3','Bonded stop pad:3',#10442,#10448,
'Bonded stop pad:3');
#226=NEXT_ASSEMBLY_USAGE_OCCURRENCE('Adjustable return-stop bracket:1',
'Adjustable return-stop bracket:1','Adjustable return-stop bracket:1',#10442,
#10449,'Adjustable return-stop bracket:1');
#227=NEXT_ASSEMBLY_USAGE_OCCURRENCE('M5x14 Cap Screw (1):2',
'M5x14 Cap Screw (1):2','M5x14 Cap Screw (1):2',#10442,#10450,
'M5x14 Cap Screw (1):2');
#228=NEXT_ASSEMBLY_USAGE_OCCURRENCE('M5x14 Cap Screw (1):3',
'M5x14 Cap Screw (1):3','M5x14 Cap Screw (1):3',#10442,#10450,
'M5x14 Cap Screw (1):3');
#229=NEXT_ASSEMBLY_USAGE_OCCURRENCE('M5x14 Cap Screw (1):4',
'M5x14 Cap Screw (1):4','M5x14 Cap Screw (1):4',#10442,#10450,
'M5x14 Cap Screw (1):4');
#230=NEXT_ASSEMBLY_USAGE_OCCURRENCE('M5x14 Cap Screw (1):5',
'M5x14 Cap Screw (1):5','M5x14 Cap Screw (1):5',#10442,#10450,
'M5x14 Cap Screw (1):5');
#231=NEXT_ASSEMBLY_USAGE_OCCURRENCE('Hex Bolt - M8x40:2',
'Hex Bolt - M8x40:2','Hex Bolt - M8x40:2',#10442,#10451,
'Hex Bolt - M8x40:2');
#232=NEXT_ASSEMBLY_USAGE_OCCURRENCE('Hex Nut - M8:2','Hex Nut - M8:2',
'Hex Nut - M8:2',#10442,#10452,'Hex Nut - M8:2');
#233=NEXT_ASSEMBLY_USAGE_OCCURRENCE(
'Compression Spring - 2.5 mm Wire, 20 mm Outside Diameter, 60 mm Long:
2',
'Compression Spring - 2.5 mm Wire, 20 mm Outside Diameter, 60 mm Long:
2',
'Compression Spring - 2.5 mm Wire, 20 mm Outside Diameter, 60 mm Long:
2',#10442,#10453,
'Compression Spring - 2.5 mm Wire, 20 mm Outside Diameter, 60 mm Long:
2');
#234=NEXT_ASSEMBLY_USAGE_OCCURRENCE('Shaft collar:2','Shaft collar:2',
'Shaft collar:2',#10442,#10454,'Shaft collar:2');
#235=NEXT_ASSEMBLY_USAGE_OCCURRENCE('Socket Set Screw - M5x8:2',
'Socket Set Screw - M5x8:2','Socket Set Screw - M5x8:2',#10442,#10455,
'Socket Set Screw - M5x8:2');
#236=NEXT_ASSEMBLY_USAGE_OCCURRENCE('Two-bushing housing:1',
'Two-bushing housing:1','Two-bushing housing:1',#10456,#10457,
'Two-bushing housing:1');
#237=NEXT_ASSEMBLY_USAGE_OCCURRENCE('Carriage table:1',
'Carriage table:1','Carriage table:1',#10456,#10458,'Carriage table:1');
#238=NEXT_ASSEMBLY_USAGE_OCCURRENCE(
'Linear Ball Bushing - 12 x 21 x 30 mm:2',
'Linear Ball Bushing - 12 x 21 x 30 mm:2',
'Linear Ball Bushing - 12 x 21 x 30 mm:2',#10456,#10459,
'Linear Ball Bushing - 12 x 21 x 30 mm:2');
#239=NEXT_ASSEMBLY_USAGE_OCCURRENCE(
'Linear Ball Bushing - 12 x 21 x 30 mm:3',
'Linear Ball Bushing - 12 x 21 x 30 mm:3',
'Linear Ball Bushing - 12 x 21 x 30 mm:3',#10456,#10459,
'Linear Ball Bushing - 12 x 21 x 30 mm:3');
#240=NEXT_ASSEMBLY_USAGE_OCCURRENCE('End retainer:2','End retainer:2',
'End retainer:2',#10456,#10462,'End retainer:2');
#241=NEXT_ASSEMBLY_USAGE_OCCURRENCE('End retainer:3','End retainer:3',
'End retainer:3',#10456,#10462,'End retainer:3');
#242=NEXT_ASSEMBLY_USAGE_OCCURRENCE('Cap Screw - M4x16:6',
'Cap Screw - M4x16:6','Cap Screw - M4x16:6',#10456,#10463,
'Cap Screw - M4x16:6');
#243=NEXT_ASSEMBLY_USAGE_OCCURRENCE('Cap Screw - M4x16:7',
'Cap Screw - M4x16:7','Cap Screw - M4x16:7',#10456,#10463,
'Cap Screw - M4x16:7');
#244=NEXT_ASSEMBLY_USAGE_OCCURRENCE('Cap Screw - M4x16:8',
'Cap Screw - M4x16:8','Cap Screw - M4x16:8',#10456,#10463,
'Cap Screw - M4x16:8');
#245=NEXT_ASSEMBLY_USAGE_OCCURRENCE('Cap Screw - M4x16:9',
'Cap Screw - M4x16:9','Cap Screw - M4x16:9',#10456,#10463,
'Cap Screw - M4x16:9');
#246=NEXT_ASSEMBLY_USAGE_OCCURRENCE('Cap Screw - M4x16:10',
'Cap Screw - M4x16:10','Cap Screw - M4x16:10',#10456,#10463,
'Cap Screw - M4x16:10');
#247=NEXT_ASSEMBLY_USAGE_OCCURRENCE('Cap Screw - M4x16:11',
'Cap Screw - M4x16:11','Cap Screw - M4x16:11',#10456,#10463,
'Cap Screw - M4x16:11');
#248=NEXT_ASSEMBLY_USAGE_OCCURRENCE('Cap Screw - M4x16:12',
'Cap Screw - M4x16:12','Cap Screw - M4x16:12',#10456,#10463,
'Cap Screw - M4x16:12');
#249=NEXT_ASSEMBLY_USAGE_OCCURRENCE('Cap Screw - M4x16:13',
'Cap Screw - M4x16:13','Cap Screw - M4x16:13',#10456,#10463,
'Cap Screw - M4x16:13');
#250=NEXT_ASSEMBLY_USAGE_OCCURRENCE('Cap Screw - M5x20:2',
'Cap Screw - M5x20:2','Cap Screw - M5x20:2',#10456,#10464,
'Cap Screw - M5x20:2');
#251=NEXT_ASSEMBLY_USAGE_OCCURRENCE('Cap Screw - M5x20:3',
'Cap Screw - M5x20:3','Cap Screw - M5x20:3',#10456,#10464,
'Cap Screw - M5x20:3');
#252=NEXT_ASSEMBLY_USAGE_OCCURRENCE('Cap Screw - M5x20:4',
'Cap Screw - M5x20:4','Cap Screw - M5x20:4',#10456,#10464,
'Cap Screw - M5x20:4');
#253=NEXT_ASSEMBLY_USAGE_OCCURRENCE('Cap Screw - M5x20:5',
'Cap Screw - M5x20:5','Cap Screw - M5x20:5',#10456,#10464,
'Cap Screw - M5x20:5');
#254=NEXT_ASSEMBLY_USAGE_OCCURRENCE('Grip:2','Grip:2','Grip:2',#10456,#10465,
'Grip:2');
#255=NEXT_ASSEMBLY_USAGE_OCCURRENCE('Flat Washer - M6:2',
'Flat Washer - M6:2','Flat Washer - M6:2',#10456,#10466,
'Flat Washer - M6:2');
#256=NEXT_ASSEMBLY_USAGE_OCCURRENCE('Cap Screw - M6x25:2',
'Cap Screw - M6x25:2','Cap Screw - M6x25:2',#10456,#10467,
'Cap Screw - M6x25:2');
#257=NEXT_ASSEMBLY_USAGE_OCCURRENCE('Shafts supports and end stops:1',
'Shafts supports and end stops:1','Shafts supports and end stops:1',#10441,
#10442,'Shafts supports and end stops:1');
#258=NEXT_ASSEMBLY_USAGE_OCCURRENCE('Two-bushing carriage:1',
'Two-bushing carriage:1','Two-bushing carriage:1',#10441,#10456,
'Two-bushing carriage:1');
#259=B_SPLINE_CURVE_WITH_KNOTS('',3,(#9348,#9349,#9350,#9351,#9352,#9353,
#9354,#9355,#9356,#9357,#9358,#9359,#9360,#9361,#9362,#9363,#9364,#9365,
#9366,#9367,#9368,#9369,#9370,#9371,#9372,#9373,#9374,#9375,#9376,#9377,
#9378,#9379,#9380,#9381,#9382,#9383,#9384,#9385,#9386,#9387,#9388,#9389,
#9390,#9391,#9392,#9393,#9394,#9395,#9396,#9397,#9398,#9399,#9400,#9401,
#9402,#9403,#9404,#9405,#9406,#9407,#9408,#9409,#9410,#9411,#9412,#9413,
#9414,#9415,#9416,#9417,#9418,#9419,#9420,#9421,#9422,#9423,#9424,#9425,
#9426,#9427,#9428,#9429,#9430,#9431,#9432,#9433,#9434,#9435,#9436,#9437,
#9438,#9439,#9440,#9441,#9442,#9443,#9444,#9445,#9446,#9447,#9448,#9449,
#9450,#9451,#9452,#9453,#9454,#9455,#9456,#9457,#9458,#9459,#9460,#9461,
#9462,#9463,#9464,#9465,#9466,#9467,#9468,#9469,#9470),.UNSPECIFIED.,.F.,
 .F.,(4,1,1,1,1,1,1,1,1,1,1,1,1,1,1,1,1,1,1,1,1,1,1,1,1,1,1,1,1,1,1,1,1,
1,1,1,1,1,1,1,1,1,1,1,1,1,1,1,1,1,1,1,1,1,1,1,1,1,1,1,1,1,1,1,1,1,1,1,1,
1,1,1,1,1,1,1,1,1,1,1,1,1,1,1,1,1,1,1,1,1,1,1,1,1,1,1,1,1,1,1,1,1,1,1,1,
1,1,1,1,1,1,1,1,1,1,1,1,1,1,1,4),(0.,0.00446428571428571,0.00892857142857143,
0.0178571428571429,0.0267857142857143,0.0357142857142857,0.0446428571428571,
0.0535714285714286,0.0625,0.0714285714285714,0.0803571428571428,0.0892857142857143,
0.0982142857142857,0.107142857142857,0.111607142857143,0.116071428571429,
0.120535714285714,0.122767857142857,0.125,0.129464285714286,0.133928571428571,
0.138392857142857,0.142857142857143,0.151785714285714,0.160714285714286,
0.169642857142857,0.174107142857143,0.178571428571429,0.1875,0.196428571428571,
0.205357142857143,0.214285714285714,0.223214285714286,0.232142857142857,
0.241071428571429,0.25,0.258928571428571,0.267857142857143,0.276785714285714,
0.285714285714286,0.294642857142857,0.303571428571429,0.3125,0.321428571428571,
0.330357142857143,0.339285714285714,0.348214285714286,0.357142857142857,
0.363095238095238,0.369047619047619,0.380952380952381,0.392857142857143,
0.401785714285714,0.410714285714286,0.419642857142857,0.428571428571429,
0.4375,0.446428571428571,0.455357142857143,0.464285714285714,0.476190476190476,
0.488095238095238,0.5,0.508928571428571,0.517857142857143,0.526785714285714,
0.535714285714286,0.544642857142857,0.553571428571429,0.5625,0.571428571428571,
0.580357142857143,0.589285714285714,0.598214285714286,0.607142857142857,
0.616071428571429,0.625,0.633928571428571,0.642857142857143,0.654761904761905,
0.666666666666667,0.678571428571428,0.6875,0.696428571428571,0.705357142857143,
0.714285714285714,0.720238095238095,0.726190476190476,0.738095238095238,
0.75,0.761904761904762,0.773809523809524,0.785714285714286,0.797619047619047,
0.809523809523809,0.821428571428571,0.833333333333333,0.845238095238095,
0.857142857142857,0.861607142857143,0.866071428571429,0.870535714285714,
0.875,0.877232142857143,0.879464285714286,0.883928571428571,0.888392857142857,
0.892857142857143,0.901785714285714,0.910714285714286,0.919642857142857,
0.928571428571429,0.9375,0.946428571428571,0.955357142857143,0.964285714285714,
0.973214285714286,0.982142857142857,0.991071428571429,0.995535714285714,
1.),.UNSPECIFIED.);
#260=B_SPLINE_CURVE_WITH_KNOTS('',3,(#9482,#9483,#9484,#9485,#9486,#9487,
#9488,#9489,#9490,#9491),.UNSPECIFIED.,.F.,.F.,(4,2,2,2,4),(0.818088904349178,
0.878131747417165,0.957937926194036,1.03774410497091,1.09778694803889),
 .UNSPECIFIED.);
#261=B_SPLINE_CURVE_WITH_KNOTS('',3,(#9497,#9498,#9499,#9500,#9501,#9502,
#9503,#9504,#9505,#9506,#9507,#9508,#9509,#9510,#9511,#9512,#9513,#9514),
 .UNSPECIFIED.,.F.,.F.,(4,2,2,2,2,2,2,2,4),(0.,0.0793157643915218,0.158631528783044,
0.237943615933649,0.317255703084255,0.396567790234861,0.475879877385467,
0.555195641776989,0.634511406168511),.UNSPECIFIED.);
#262=B_SPLINE_CURVE_WITH_KNOTS('',3,(#9515,#9516,#9517,#9518,#9519,#9520,
#9521,#9522,#9523,#9524,#9525,#9526,#9527,#9528,#9529,#9530,#9531,#9532),
 .UNSPECIFIED.,.F.,.F.,(4,2,2,2,2,2,2,2,4),(0.634511406168511,0.713827170560032,
0.793142934951554,0.87245502210216,0.951767109252766,1.03107919640337,1.11039128355398,
1.1897070479455,1.26902281233702),.UNSPECIFIED.);
#263=B_SPLINE_CURVE_WITH_KNOTS('',3,(#9535,#9536,#9537,#9538,#9539,#9540,
#9541,#9542,#9543,#9544),.UNSPECIFIED.,.F.,.F.,(4,2,2,2,4),(0.17946362021982,
0.239506463287808,0.319312642064679,0.39911882084155,0.459161663909536),
 .UNSPECIFIED.);
#264=B_SPLINE_SURFACE_WITH_KNOTS('',3,3,((#8115,#8116,#8117,#8118,#8119,
#8120,#8121,#8122,#8123,#8124,#8125,#8126,#8127,#8128,#8129,#8130,#8131,
#8132,#8133,#8134,#8135,#8136,#8137,#8138,#8139,#8140,#8141,#8142,#8143,
#8144,#8145,#8146,#8147,#8148,#8149,#8150,#8151,#8152,#8153,#8154,#8155,
#8156,#8157,#8158,#8159,#8160,#8161,#8162,#8163,#8164,#8165,#8166,#8167,
#8168,#8169,#8170,#8171,#8172,#8173,#8174,#8175,#8176,#8177,#8178,#8179,
#8180,#8181,#8182,#8183,#8184,#8185,#8186,#8187,#8188,#8189,#8190,#8191,
#8192,#8193,#8194,#8195,#8196,#8197,#8198,#8199,#8200,#8201,#8202,#8203,
#8204,#8205,#8206,#8207,#8208,#8209,#8210,#8211,#8212,#8213,#8214,#8215,
#8216,#8217,#8218,#8219,#8220,#8221,#8222,#8223,#8224,#8225,#8226,#8227,
#8228,#8229,#8230,#8231,#8232,#8233,#8234,#8235,#8236,#8237),(#8238,#8239,
#8240,#8241,#8242,#8243,#8244,#8245,#8246,#8247,#8248,#8249,#8250,#8251,
#8252,#8253,#8254,#8255,#8256,#8257,#8258,#8259,#8260,#8261,#8262,#8263,
#8264,#8265,#8266,#8267,#8268,#8269,#8270,#8271,#8272,#8273,#8274,#8275,
#8276,#8277,#8278,#8279,#8280,#8281,#8282,#8283,#8284,#8285,#8286,#8287,
#8288,#8289,#8290,#8291,#8292,#8293,#8294,#8295,#8296,#8297,#8298,#8299,
#8300,#8301,#8302,#8303,#8304,#8305,#8306,#8307,#8308,#8309,#8310,#8311,
#8312,#8313,#8314,#8315,#8316,#8317,#8318,#8319,#8320,#8321,#8322,#8323,
#8324,#8325,#8326,#8327,#8328,#8329,#8330,#8331,#8332,#8333,#8334,#8335,
#8336,#8337,#8338,#8339,#8340,#8341,#8342,#8343,#8344,#8345,#8346,#8347,
#8348,#8349,#8350,#8351,#8352,#8353,#8354,#8355,#8356,#8357,#8358,#8359,
#8360),(#8361,#8362,#8363,#8364,#8365,#8366,#8367,#8368,#8369,#8370,#8371,
#8372,#8373,#8374,#8375,#8376,#8377,#8378,#8379,#8380,#8381,#8382,#8383,
#8384,#8385,#8386,#8387,#8388,#8389,#8390,#8391,#8392,#8393,#8394,#8395,
#8396,#8397,#8398,#8399,#8400,#8401,#8402,#8403,#8404,#8405,#8406,#8407,
#8408,#8409,#8410,#8411,#8412,#8413,#8414,#8415,#8416,#8417,#8418,#8419,
#8420,#8421,#8422,#8423,#8424,#8425,#8426,#8427,#8428,#8429,#8430,#8431,
#8432,#8433,#8434,#8435,#8436,#8437,#8438,#8439,#8440,#8441,#8442,#8443,
#8444,#8445,#8446,#8447,#8448,#8449,#8450,#8451,#8452,#8453,#8454,#8455,
#8456,#8457,#8458,#8459,#8460,#8461,#8462,#8463,#8464,#8465,#8466,#8467,
#8468,#8469,#8470,#8471,#8472,#8473,#8474,#8475,#8476,#8477,#8478,#8479,
#8480,#8481,#8482,#8483),(#8484,#8485,#8486,#8487,#8488,#8489,#8490,#8491,
#8492,#8493,#8494,#8495,#8496,#8497,#8498,#8499,#8500,#8501,#8502,#8503,
#8504,#8505,#8506,#8507,#8508,#8509,#8510,#8511,#8512,#8513,#8514,#8515,
#8516,#8517,#8518,#8519,#8520,#8521,#8522,#8523,#8524,#8525,#8526,#8527,
#8528,#8529,#8530,#8531,#8532,#8533,#8534,#8535,#8536,#8537,#8538,#8539,
#8540,#8541,#8542,#8543,#8544,#8545,#8546,#8547,#8548,#8549,#8550,#8551,
#8552,#8553,#8554,#8555,#8556,#8557,#8558,#8559,#8560,#8561,#8562,#8563,
#8564,#8565,#8566,#8567,#8568,#8569,#8570,#8571,#8572,#8573,#8574,#8575,
#8576,#8577,#8578,#8579,#8580,#8581,#8582,#8583,#8584,#8585,#8586,#8587,
#8588,#8589,#8590,#8591,#8592,#8593,#8594,#8595,#8596,#8597,#8598,#8599,
#8600,#8601,#8602,#8603,#8604,#8605,#8606),(#8607,#8608,#8609,#8610,#8611,
#8612,#8613,#8614,#8615,#8616,#8617,#8618,#8619,#8620,#8621,#8622,#8623,
#8624,#8625,#8626,#8627,#8628,#8629,#8630,#8631,#8632,#8633,#8634,#8635,
#8636,#8637,#8638,#8639,#8640,#8641,#8642,#8643,#8644,#8645,#8646,#8647,
#8648,#8649,#8650,#8651,#8652,#8653,#8654,#8655,#8656,#8657,#8658,#8659,
#8660,#8661,#8662,#8663,#8664,#8665,#8666,#8667,#8668,#8669,#8670,#8671,
#8672,#8673,#8674,#8675,#8676,#8677,#8678,#8679,#8680,#8681,#8682,#8683,
#8684,#8685,#8686,#8687,#8688,#8689,#8690,#8691,#8692,#8693,#8694,#8695,
#8696,#8697,#8698,#8699,#8700,#8701,#8702,#8703,#8704,#8705,#8706,#8707,
#8708,#8709,#8710,#8711,#8712,#8713,#8714,#8715,#8716,#8717,#8718,#8719,
#8720,#8721,#8722,#8723,#8724,#8725,#8726,#8727,#8728,#8729),(#8730,#8731,
#8732,#8733,#8734,#8735,#8736,#8737,#8738,#8739,#8740,#8741,#8742,#8743,
#8744,#8745,#8746,#8747,#8748,#8749,#8750,#8751,#8752,#8753,#8754,#8755,
#8756,#8757,#8758,#8759,#8760,#8761,#8762,#8763,#8764,#8765,#8766,#8767,
#8768,#8769,#8770,#8771,#8772,#8773,#8774,#8775,#8776,#8777,#8778,#8779,
#8780,#8781,#8782,#8783,#8784,#8785,#8786,#8787,#8788,#8789,#8790,#8791,
#8792,#8793,#8794,#8795,#8796,#8797,#8798,#8799,#8800,#8801,#8802,#8803,
#8804,#8805,#8806,#8807,#8808,#8809,#8810,#8811,#8812,#8813,#8814,#8815,
#8816,#8817,#8818,#8819,#8820,#8821,#8822,#8823,#8824,#8825,#8826,#8827,
#8828,#8829,#8830,#8831,#8832,#8833,#8834,#8835,#8836,#8837,#8838,#8839,
#8840,#8841,#8842,#8843,#8844,#8845,#8846,#8847,#8848,#8849,#8850,#8851,
#8852),(#8853,#8854,#8855,#8856,#8857,#8858,#8859,#8860,#8861,#8862,#8863,
#8864,#8865,#8866,#8867,#8868,#8869,#8870,#8871,#8872,#8873,#8874,#8875,
#8876,#8877,#8878,#8879,#8880,#8881,#8882,#8883,#8884,#8885,#8886,#8887,
#8888,#8889,#8890,#8891,#8892,#8893,#8894,#8895,#8896,#8897,#8898,#8899,
#8900,#8901,#8902,#8903,#8904,#8905,#8906,#8907,#8908,#8909,#8910,#8911,
#8912,#8913,#8914,#8915,#8916,#8917,#8918,#8919,#8920,#8921,#8922,#8923,
#8924,#8925,#8926,#8927,#8928,#8929,#8930,#8931,#8932,#8933,#8934,#8935,
#8936,#8937,#8938,#8939,#8940,#8941,#8942,#8943,#8944,#8945,#8946,#8947,
#8948,#8949,#8950,#8951,#8952,#8953,#8954,#8955,#8956,#8957,#8958,#8959,
#8960,#8961,#8962,#8963,#8964,#8965,#8966,#8967,#8968,#8969,#8970,#8971,
#8972,#8973,#8974,#8975),(#8976,#8977,#8978,#8979,#8980,#8981,#8982,#8983,
#8984,#8985,#8986,#8987,#8988,#8989,#8990,#8991,#8992,#8993,#8994,#8995,
#8996,#8997,#8998,#8999,#9000,#9001,#9002,#9003,#9004,#9005,#9006,#9007,
#9008,#9009,#9010,#9011,#9012,#9013,#9014,#9015,#9016,#9017,#9018,#9019,
#9020,#9021,#9022,#9023,#9024,#9025,#9026,#9027,#9028,#9029,#9030,#9031,
#9032,#9033,#9034,#9035,#9036,#9037,#9038,#9039,#9040,#9041,#9042,#9043,
#9044,#9045,#9046,#9047,#9048,#9049,#9050,#9051,#9052,#9053,#9054,#9055,
#9056,#9057,#9058,#9059,#9060,#9061,#9062,#9063,#9064,#9065,#9066,#9067,
#9068,#9069,#9070,#9071,#9072,#9073,#9074,#9075,#9076,#9077,#9078,#9079,
#9080,#9081,#9082,#9083,#9084,#9085,#9086,#9087,#9088,#9089,#9090,#9091,
#9092,#9093,#9094,#9095,#9096,#9097,#9098),(#9099,#9100,#9101,#9102,#9103,
#9104,#9105,#9106,#9107,#9108,#9109,#9110,#9111,#9112,#9113,#9114,#9115,
#9116,#9117,#9118,#9119,#9120,#9121,#9122,#9123,#9124,#9125,#9126,#9127,
#9128,#9129,#9130,#9131,#9132,#9133,#9134,#9135,#9136,#9137,#9138,#9139,
#9140,#9141,#9142,#9143,#9144,#9145,#9146,#9147,#9148,#9149,#9150,#9151,
#9152,#9153,#9154,#9155,#9156,#9157,#9158,#9159,#9160,#9161,#9162,#9163,
#9164,#9165,#9166,#9167,#9168,#9169,#9170,#9171,#9172,#9173,#9174,#9175,
#9176,#9177,#9178,#9179,#9180,#9181,#9182,#9183,#9184,#9185,#9186,#9187,
#9188,#9189,#9190,#9191,#9192,#9193,#9194,#9195,#9196,#9197,#9198,#9199,
#9200,#9201,#9202,#9203,#9204,#9205,#9206,#9207,#9208,#9209,#9210,#9211,
#9212,#9213,#9214,#9215,#9216,#9217,#9218,#9219,#9220,#9221),(#9222,#9223,
#9224,#9225,#9226,#9227,#9228,#9229,#9230,#9231,#9232,#9233,#9234,#9235,
#9236,#9237,#9238,#9239,#9240,#9241,#9242,#9243,#9244,#9245,#9246,#9247,
#9248,#9249,#9250,#9251,#9252,#9253,#9254,#9255,#9256,#9257,#9258,#9259,
#9260,#9261,#9262,#9263,#9264,#9265,#9266,#9267,#9268,#9269,#9270,#9271,
#9272,#9273,#9274,#9275,#9276,#9277,#9278,#9279,#9280,#9281,#9282,#9283,
#9284,#9285,#9286,#9287,#9288,#9289,#9290,#9291,#9292,#9293,#9294,#9295,
#9296,#9297,#9298,#9299,#9300,#9301,#9302,#9303,#9304,#9305,#9306,#9307,
#9308,#9309,#9310,#9311,#9312,#9313,#9314,#9315,#9316,#9317,#9318,#9319,
#9320,#9321,#9322,#9323,#9324,#9325,#9326,#9327,#9328,#9329,#9330,#9331,
#9332,#9333,#9334,#9335,#9336,#9337,#9338,#9339,#9340,#9341,#9342,#9343,
#9344)),.UNSPECIFIED.,.T.,.F.,.F.,(4,1,1,1,1,1,1,4),(4,1,1,1,1,1,1,1,1,
1,1,1,1,1,1,1,1,1,1,1,1,1,1,1,1,1,1,1,1,1,1,1,1,1,1,1,1,1,1,1,1,1,1,1,1,
1,1,1,1,1,1,1,1,1,1,1,1,1,1,1,1,1,1,1,1,1,1,1,1,1,1,1,1,1,1,1,1,1,1,1,1,
1,1,1,1,1,1,1,1,1,1,1,1,1,1,1,1,1,1,1,1,1,1,1,1,1,1,1,1,1,1,1,1,1,1,1,1,
1,1,1,4),(-3.14159265358979,-2.24399475256414,-1.34639685153848,-0.448798950512828,
0.448798950512828,1.34639685153848,2.24399475256414,3.14159265358979),(0.,
0.00446428571428571,0.00892857142857143,0.0178571428571429,0.0267857142857143,
0.0357142857142857,0.0446428571428571,0.0535714285714286,0.0625,0.0714285714285714,
0.0803571428571428,0.0892857142857143,0.0982142857142857,0.107142857142857,
0.111607142857143,0.116071428571429,0.120535714285714,0.122767857142857,
0.125,0.129464285714286,0.133928571428571,0.138392857142857,0.142857142857143,
0.151785714285714,0.160714285714286,0.169642857142857,0.174107142857143,
0.178571428571429,0.1875,0.196428571428571,0.205357142857143,0.214285714285714,
0.223214285714286,0.232142857142857,0.241071428571429,0.25,0.258928571428571,
0.267857142857143,0.276785714285714,0.285714285714286,0.294642857142857,
0.303571428571429,0.3125,0.321428571428571,0.330357142857143,0.339285714285714,
0.348214285714286,0.357142857142857,0.363095238095238,0.369047619047619,
0.380952380952381,0.392857142857143,0.401785714285714,0.410714285714286,
0.419642857142857,0.428571428571429,0.4375,0.446428571428571,0.455357142857143,
0.464285714285714,0.476190476190476,0.488095238095238,0.5,0.508928571428571,
0.517857142857143,0.526785714285714,0.535714285714286,0.544642857142857,
0.553571428571429,0.5625,0.571428571428571,0.580357142857143,0.589285714285714,
0.598214285714286,0.607142857142857,0.616071428571429,0.625,0.633928571428571,
0.642857142857143,0.654761904761905,0.666666666666667,0.678571428571428,
0.6875,0.696428571428571,0.705357142857143,0.714285714285714,0.720238095238095,
0.726190476190476,0.738095238095238,0.75,0.761904761904762,0.773809523809524,
0.785714285714286,0.797619047619047,0.809523809523809,0.821428571428571,
0.833333333333333,0.845238095238095,0.857142857142857,0.861607142857143,
0.866071428571429,0.870535714285714,0.875,0.877232142857143,0.879464285714286,
0.883928571428571,0.888392857142857,0.892857142857143,0.901785714285714,
0.910714285714286,0.919642857142857,0.928571428571429,0.9375,0.946428571428571,
0.955357142857143,0.964285714285714,0.973214285714286,0.982142857142857,
0.991071428571429,0.995535714285714,1.),.UNSPECIFIED.);
#265=(
BOUNDED_CURVE()
B_SPLINE_CURVE(2,(#7989,#7990,#7991),.UNSPECIFIED.,.F.,.F.)
B_SPLINE_CURVE_WITH_KNOTS((3,3),(0.14973948338295,0.97160236658079),
 .UNSPECIFIED.)
CURVE()
GEOMETRIC_REPRESENTATION_ITEM()
RATIONAL_B_SPLINE_CURVE((1.07140024848292,1.23714644374248,1.07140024848292))
REPRESENTATION_ITEM('')
);
#266=(
BOUNDED_CURVE()
B_SPLINE_CURVE(2,(#7993,#7994,#7995),.UNSPECIFIED.,.F.,.F.)
B_SPLINE_CURVE_WITH_KNOTS((3,3),(0.14973948338295,0.97160236658079),
 .UNSPECIFIED.)
CURVE()
GEOMETRIC_REPRESENTATION_ITEM()
RATIONAL_B_SPLINE_CURVE((1.07140024848292,1.23714644374248,1.07140024848292))
REPRESENTATION_ITEM('')
);
#267=(
BOUNDED_CURVE()
B_SPLINE_CURVE(2,(#7997,#7998,#7999),.UNSPECIFIED.,.F.,.F.)
B_SPLINE_CURVE_WITH_KNOTS((3,3),(0.14973948338295,0.97160236658079),
 .UNSPECIFIED.)
CURVE()
GEOMETRIC_REPRESENTATION_ITEM()
RATIONAL_B_SPLINE_CURVE((1.07140024848292,1.23714644374248,1.07140024848292))
REPRESENTATION_ITEM('')
);
#268=(
BOUNDED_CURVE()
B_SPLINE_CURVE(2,(#8001,#8002,#8003),.UNSPECIFIED.,.F.,.F.)
B_SPLINE_CURVE_WITH_KNOTS((3,3),(0.149739483382949,0.971602366580789),
 .UNSPECIFIED.)
CURVE()
GEOMETRIC_REPRESENTATION_ITEM()
RATIONAL_B_SPLINE_CURVE((1.07140024848292,1.23714644374248,1.07140024848292))
REPRESENTATION_ITEM('')
);
#269=(
BOUNDED_CURVE()
B_SPLINE_CURVE(2,(#8005,#8006,#8007),.UNSPECIFIED.,.F.,.F.)
B_SPLINE_CURVE_WITH_KNOTS((3,3),(0.14973948338295,0.971602366580789),
 .UNSPECIFIED.)
CURVE()
GEOMETRIC_REPRESENTATION_ITEM()
RATIONAL_B_SPLINE_CURVE((1.07140024848292,1.23714644374248,1.07140024848292))
REPRESENTATION_ITEM('')
);
#270=(
BOUNDED_CURVE()
B_SPLINE_CURVE(2,(#8008,#8009,#8010),.UNSPECIFIED.,.F.,.F.)
B_SPLINE_CURVE_WITH_KNOTS((3,3),(0.14973948338295,0.97160236658079),
 .UNSPECIFIED.)
CURVE()
GEOMETRIC_REPRESENTATION_ITEM()
RATIONAL_B_SPLINE_CURVE((1.07140024848292,1.23714644374248,1.07140024848292))
REPRESENTATION_ITEM('')
);
#271=(
BOUNDED_CURVE()
B_SPLINE_CURVE(2,(#8041,#8042,#8043),.UNSPECIFIED.,.F.,.F.)
B_SPLINE_CURVE_WITH_KNOTS((3,3),(0.14973948338295,0.97160236658079),
 .UNSPECIFIED.)
CURVE()
GEOMETRIC_REPRESENTATION_ITEM()
RATIONAL_B_SPLINE_CURVE((1.07140024848292,1.23714644374248,1.07140024848292))
REPRESENTATION_ITEM('')
);
#272=(
BOUNDED_CURVE()
B_SPLINE_CURVE(2,(#8045,#8046,#8047),.UNSPECIFIED.,.F.,.F.)
B_SPLINE_CURVE_WITH_KNOTS((3,3),(0.14973948338295,0.971602366580789),
 .UNSPECIFIED.)
CURVE()
GEOMETRIC_REPRESENTATION_ITEM()
RATIONAL_B_SPLINE_CURVE((1.07140024848292,1.23714644374248,1.07140024848292))
REPRESENTATION_ITEM('')
);
#273=(
BOUNDED_CURVE()
B_SPLINE_CURVE(2,(#8052,#8053,#8054),.UNSPECIFIED.,.F.,.F.)
B_SPLINE_CURVE_WITH_KNOTS((3,3),(0.14973948338295,0.97160236658079),
 .UNSPECIFIED.)
CURVE()
GEOMETRIC_REPRESENTATION_ITEM()
RATIONAL_B_SPLINE_CURVE((1.07140024848292,1.23714644374248,1.07140024848292))
REPRESENTATION_ITEM('')
);
#274=(
BOUNDED_CURVE()
B_SPLINE_CURVE(2,(#8056,#8057,#8058),.UNSPECIFIED.,.F.,.F.)
B_SPLINE_CURVE_WITH_KNOTS((3,3),(0.14973948338295,0.97160236658079),
 .UNSPECIFIED.)
CURVE()
GEOMETRIC_REPRESENTATION_ITEM()
RATIONAL_B_SPLINE_CURVE((1.07140024848292,1.23714644374248,1.07140024848292))
REPRESENTATION_ITEM('')
);
#275=(
BOUNDED_CURVE()
B_SPLINE_CURVE(2,(#8060,#8061,#8062),.UNSPECIFIED.,.F.,.F.)
B_SPLINE_CURVE_WITH_KNOTS((3,3),(0.14973948338295,0.971602366580789),
 .UNSPECIFIED.)
CURVE()
GEOMETRIC_REPRESENTATION_ITEM()
RATIONAL_B_SPLINE_CURVE((1.07140024848292,1.23714644374248,1.07140024848292))
REPRESENTATION_ITEM('')
);
#276=(
BOUNDED_CURVE()
B_SPLINE_CURVE(2,(#8063,#8064,#8065),.UNSPECIFIED.,.F.,.F.)
B_SPLINE_CURVE_WITH_KNOTS((3,3),(0.14973948338295,0.97160236658079),
 .UNSPECIFIED.)
CURVE()
GEOMETRIC_REPRESENTATION_ITEM()
RATIONAL_B_SPLINE_CURVE((1.07140024848292,1.23714644374248,1.07140024848292))
REPRESENTATION_ITEM('')
);
#277=(
BOUNDED_CURVE()
B_SPLINE_CURVE(2,(#8072,#8073,#8074),.UNSPECIFIED.,.F.,.F.)
B_SPLINE_CURVE_WITH_KNOTS((3,3),(0.14973948338295,0.97160236658079),
 .UNSPECIFIED.)
CURVE()
GEOMETRIC_REPRESENTATION_ITEM()
RATIONAL_B_SPLINE_CURVE((1.07140024848292,1.23714644374248,1.07140024848292))
REPRESENTATION_ITEM('')
);
#278=(
BOUNDED_CURVE()
B_SPLINE_CURVE(2,(#8076,#8077,#8078),.UNSPECIFIED.,.F.,.F.)
B_SPLINE_CURVE_WITH_KNOTS((3,3),(0.14973948338295,0.97160236658079),
 .UNSPECIFIED.)
CURVE()
GEOMETRIC_REPRESENTATION_ITEM()
RATIONAL_B_SPLINE_CURVE((1.07140024848292,1.23714644374248,1.07140024848292))
REPRESENTATION_ITEM('')
);
#279=(
BOUNDED_CURVE()
B_SPLINE_CURVE(2,(#8080,#8081,#8082),.UNSPECIFIED.,.F.,.F.)
B_SPLINE_CURVE_WITH_KNOTS((3,3),(0.14973948338295,0.971602366580789),
 .UNSPECIFIED.)
CURVE()
GEOMETRIC_REPRESENTATION_ITEM()
RATIONAL_B_SPLINE_CURVE((1.07140024848292,1.23714644374248,1.07140024848292))
REPRESENTATION_ITEM('')
);
#280=(
BOUNDED_CURVE()
B_SPLINE_CURVE(2,(#8084,#8085,#8086),.UNSPECIFIED.,.F.,.F.)
B_SPLINE_CURVE_WITH_KNOTS((3,3),(0.14973948338295,0.97160236658079),
 .UNSPECIFIED.)
CURVE()
GEOMETRIC_REPRESENTATION_ITEM()
RATIONAL_B_SPLINE_CURVE((1.07140024848292,1.23714644374248,1.07140024848292))
REPRESENTATION_ITEM('')
);
#281=(
BOUNDED_CURVE()
B_SPLINE_CURVE(2,(#8088,#8089,#8090),.UNSPECIFIED.,.F.,.F.)
B_SPLINE_CURVE_WITH_KNOTS((3,3),(0.14973948338295,0.97160236658079),
 .UNSPECIFIED.)
CURVE()
GEOMETRIC_REPRESENTATION_ITEM()
RATIONAL_B_SPLINE_CURVE((1.07140024848292,1.23714644374248,1.07140024848292))
REPRESENTATION_ITEM('')
);
#282=(
BOUNDED_CURVE()
B_SPLINE_CURVE(2,(#8091,#8092,#8093),.UNSPECIFIED.,.F.,.F.)
B_SPLINE_CURVE_WITH_KNOTS((3,3),(0.14973948338295,0.971602366580789),
 .UNSPECIFIED.)
CURVE()
GEOMETRIC_REPRESENTATION_ITEM()
RATIONAL_B_SPLINE_CURVE((1.07140024848292,1.23714644374248,1.07140024848292))
REPRESENTATION_ITEM('')
);
#283=ORIENTED_CLOSED_SHELL('',*,#5010,.F.);
#284=ORIENTED_CLOSED_SHELL('',*,#5015,.F.);
#285=ORIENTED_CLOSED_SHELL('',*,#5028,.F.);
#286=ORIENTED_CLOSED_SHELL('',*,#5030,.F.);
#287=ORIENTED_CLOSED_SHELL('',*,#5034,.F.);
#288=BREP_WITH_VOIDS('Body1',#5011,(#283));
#289=BREP_WITH_VOIDS('Body1',#5016,(#284));
#290=BREP_WITH_VOIDS('Body1',#5027,(#285));
#291=BREP_WITH_VOIDS('Body1',#5029,(#286));
#292=BREP_WITH_VOIDS('Body1',#5033,(#287));
#293=CONICAL_SURFACE('',#5347,0.55,0.785398163397448);
#294=CONICAL_SURFACE('',#5353,0.55,0.785398163397441);
#295=CONICAL_SURFACE('',#5407,0.4,0.785398163397448);
#296=CONICAL_SURFACE('',#5411,0.41,0.785398163397448);
#297=CONICAL_SURFACE('',#5415,0.26,0.463647609000806);
#298=CONICAL_SURFACE('',#5486,0.4,0.785398163397448);
#299=CONICAL_SURFACE('',#5490,0.41,0.785398163397448);
#300=CONICAL_SURFACE('',#5494,0.26,0.463647609000806);
#301=CONICAL_SURFACE('',#5501,0.36,0.785398163397451);
#302=CONICAL_SURFACE('',#5504,0.734027674973257,1.0471975511966);
#303=CONICAL_SURFACE('',#5515,0.734027674973257,1.0471975511966);
#304=CONICAL_SURFACE('',#5517,0.734027674973257,1.0471975511966);
#305=CONICAL_SURFACE('',#5560,0.235,0.785398163397448);
#306=CONICAL_SURFACE('',#5564,0.2125,0.785398163397448);
#307=CONICAL_SURFACE('',#5711,0.325,0.785398163397448);
#308=CONICAL_SURFACE('',#5715,0.335,0.785398163397448);
#309=CONICAL_SURFACE('',#5719,0.21,0.463647609000806);
#310=CONICAL_SURFACE('',#5723,0.18,0.785398163397448);
#311=CONICAL_SURFACE('',#5737,0.4,0.785398163397448);
#312=CONICAL_SURFACE('',#5741,0.41,0.785398163397448);
#313=CONICAL_SURFACE('',#5745,0.26,0.463647609000806);
#314=CONICAL_SURFACE('',#5749,0.225,0.785398163397448);
#315=CONICAL_SURFACE('',#5818,0.475,0.785398163397449);
#316=CONICAL_SURFACE('',#5822,0.485,0.785398163397448);
#317=CONICAL_SURFACE('',#5826,0.31,0.463647609000806);
#318=CONICAL_SURFACE('',#5830,0.27,0.785398163397448);
#319=SHAPE_REPRESENTATION_RELATIONSHIP('SRR','None',#10415,#342);
#320=SHAPE_REPRESENTATION_RELATIONSHIP('SRR','None',#10416,#343);
#321=SHAPE_REPRESENTATION_RELATIONSHIP('SRR','None',#10417,#344);
#322=SHAPE_REPRESENTATION_RELATIONSHIP('SRR','None',#10418,#345);
#323=SHAPE_REPRESENTATION_RELATIONSHIP('SRR','None',#10419,#346);
#324=SHAPE_REPRESENTATION_RELATIONSHIP('SRR','None',#10420,#347);
#325=SHAPE_REPRESENTATION_RELATIONSHIP('SRR','None',#10421,#348);
#326=SHAPE_REPRESENTATION_RELATIONSHIP('SRR','None',#10422,#349);
#327=SHAPE_REPRESENTATION_RELATIONSHIP('SRR','None',#10423,#350);
#328=SHAPE_REPRESENTATION_RELATIONSHIP('SRR','None',#10424,#351);
#329=SHAPE_REPRESENTATION_RELATIONSHIP('SRR','None',#10425,#352);
#330=SHAPE_REPRESENTATION_RELATIONSHIP('SRR','None',#10426,#353);
#331=SHAPE_REPRESENTATION_RELATIONSHIP('SRR','None',#10427,#354);
#332=SHAPE_REPRESENTATION_RELATIONSHIP('SRR','None',#10429,#355);
#333=SHAPE_REPRESENTATION_RELATIONSHIP('SRR','None',#10430,#356);
#334=SHAPE_REPRESENTATION_RELATIONSHIP('SRR','None',#10432,#357);
#335=SHAPE_REPRESENTATION_RELATIONSHIP('SRR','None',#10433,#358);
#336=SHAPE_REPRESENTATION_RELATIONSHIP('SRR','None',#10434,#359);
#337=SHAPE_REPRESENTATION_RELATIONSHIP('SRR','None',#10435,#360);
#338=SHAPE_REPRESENTATION_RELATIONSHIP('SRR','None',#10436,#361);
#339=SHAPE_REPRESENTATION_RELATIONSHIP('SRR','None',#10437,#362);
#340=SHAPE_REPRESENTATION_RELATIONSHIP('SRR','None',#10438,#363);
#341=SHAPE_REPRESENTATION_RELATIONSHIP('SRR','None',#10439,#364);
#342=ADVANCED_BREP_SHAPE_REPRESENTATION('',(#388),#10267);
#343=ADVANCED_BREP_SHAPE_REPRESENTATION('',(#389),#10268);
#344=ADVANCED_BREP_SHAPE_REPRESENTATION('',(#390),#10269);
#345=ADVANCED_BREP_SHAPE_REPRESENTATION('',(#288),#10270);
#346=ADVANCED_BREP_SHAPE_REPRESENTATION('',(#391),#10271);
#347=ADVANCED_BREP_SHAPE_REPRESENTATION('',(#392),#10272);
#348=ADVANCED_BREP_SHAPE_REPRESENTATION('',(#393),#10273);
#349=ADVANCED_BREP_SHAPE_REPRESENTATION('',(#289),#10274);
#350=ADVANCED_BREP_SHAPE_REPRESENTATION('',(#394),#10275);
#351=ADVANCED_BREP_SHAPE_REPRESENTATION('',(#395),#10276);
#352=ADVANCED_BREP_SHAPE_REPRESENTATION('',(#396),#10277);
#353=ADVANCED_BREP_SHAPE_REPRESENTATION('',(#397),#10278);
#354=ADVANCED_BREP_SHAPE_REPRESENTATION('',(#398),#10279);
#355=ADVANCED_BREP_SHAPE_REPRESENTATION('',(#399),#10281);
#356=ADVANCED_BREP_SHAPE_REPRESENTATION('',(#400),#10282);
#357=ADVANCED_BREP_SHAPE_REPRESENTATION('',(#401),#10284);
#358=ADVANCED_BREP_SHAPE_REPRESENTATION('',(#402),#10285);
#359=ADVANCED_BREP_SHAPE_REPRESENTATION('',(#403),#10286);
#360=ADVANCED_BREP_SHAPE_REPRESENTATION('',(#290),#10287);
#361=ADVANCED_BREP_SHAPE_REPRESENTATION('',(#291),#10288);
#362=ADVANCED_BREP_SHAPE_REPRESENTATION('',(#404),#10289);
#363=ADVANCED_BREP_SHAPE_REPRESENTATION('',(#405),#10290);
#364=ADVANCED_BREP_SHAPE_REPRESENTATION('',(#292),#10291);
#365=STYLED_ITEM('',(#10607),#388);
#366=STYLED_ITEM('',(#10628),#389);
#367=STYLED_ITEM('',(#10628),#390);
#368=STYLED_ITEM('',(#10635),#288);
#369=STYLED_ITEM('',(#10621),#391);
#370=STYLED_ITEM('',(#10642),#392);
#371=STYLED_ITEM('',(#10607),#393);
#372=STYLED_ITEM('',(#10635),#289);
#373=STYLED_ITEM('',(#10635),#394);
#374=STYLED_ITEM('',(#10635),#395);
#375=STYLED_ITEM('',(#10628),#396);
#376=STYLED_ITEM('',(#10628),#397);
#377=STYLED_ITEM('',(#10635),#398);
#378=STYLED_ITEM('',(#10607),#399);
#379=STYLED_ITEM('',(#10621),#400);
#380=STYLED_ITEM('',(#10642),#401);
#381=STYLED_ITEM('',(#10621),#402);
#382=STYLED_ITEM('',(#10614),#403);
#383=STYLED_ITEM('',(#10635),#290);
#384=STYLED_ITEM('',(#10635),#291);
#385=STYLED_ITEM('',(#10635),#404);
#386=STYLED_ITEM('',(#10635),#405);
#387=STYLED_ITEM('',(#10635),#292);
#388=MANIFOLD_SOLID_BREP('Body1',#5007);
#389=MANIFOLD_SOLID_BREP('Body1',#5008);
#390=MANIFOLD_SOLID_BREP('Body1',#5009);
#391=MANIFOLD_SOLID_BREP('Body1',#5012);
#392=MANIFOLD_SOLID_BREP('Body1',#5013);
#393=MANIFOLD_SOLID_BREP('Body1',#5014);
#394=MANIFOLD_SOLID_BREP('Body1',#5017);
#395=MANIFOLD_SOLID_BREP('Body1',#5018);
#396=MANIFOLD_SOLID_BREP('Body1',#5019);
#397=MANIFOLD_SOLID_BREP('Body1',#5020);
#398=MANIFOLD_SOLID_BREP('Body1',#5021);
#399=MANIFOLD_SOLID_BREP('Body1',#5022);
#400=MANIFOLD_SOLID_BREP('Body1',#5023);
#401=MANIFOLD_SOLID_BREP('Body1',#5024);
#402=MANIFOLD_SOLID_BREP('Body1',#5025);
#403=MANIFOLD_SOLID_BREP('Body1',#5026);
#404=MANIFOLD_SOLID_BREP('Body1',#5031);
#405=MANIFOLD_SOLID_BREP('Body1',#5032);
#406=FACE_BOUND('',#1019,.T.);
#407=FACE_BOUND('',#1020,.T.);
#408=FACE_BOUND('',#1021,.T.);
#409=FACE_BOUND('',#1022,.T.);
#410=FACE_BOUND('',#1023,.T.);
#411=FACE_BOUND('',#1024,.T.);
#412=FACE_BOUND('',#1025,.T.);
#413=FACE_BOUND('',#1026,.T.);
#414=FACE_BOUND('',#1027,.T.);
#415=FACE_BOUND('',#1028,.T.);
#416=FACE_BOUND('',#1029,.T.);
#417=FACE_BOUND('',#1030,.T.);
#418=FACE_BOUND('',#1031,.T.);
#419=FACE_BOUND('',#1032,.T.);
#420=FACE_BOUND('',#1033,.T.);
#421=FACE_BOUND('',#1034,.T.);
#422=FACE_BOUND('',#1036,.T.);
#423=FACE_BOUND('',#1037,.T.);
#424=FACE_BOUND('',#1038,.T.);
#425=FACE_BOUND('',#1039,.T.);
#426=FACE_BOUND('',#1040,.T.);
#427=FACE_BOUND('',#1041,.T.);
#428=FACE_BOUND('',#1042,.T.);
#429=FACE_BOUND('',#1043,.T.);
#430=FACE_BOUND('',#1044,.T.);
#431=FACE_BOUND('',#1045,.T.);
#432=FACE_BOUND('',#1046,.T.);
#433=FACE_BOUND('',#1047,.T.);
#434=FACE_BOUND('',#1048,.T.);
#435=FACE_BOUND('',#1049,.T.);
#436=FACE_BOUND('',#1050,.T.);
#437=FACE_BOUND('',#1051,.T.);
#438=FACE_BOUND('',#1062,.T.);
#439=FACE_BOUND('',#1064,.T.);
#440=FACE_BOUND('',#1066,.T.);
#441=FACE_BOUND('',#1073,.T.);
#442=FACE_BOUND('',#1076,.T.);
#443=FACE_BOUND('',#1077,.T.);
#444=FACE_BOUND('',#1080,.T.);
#445=FACE_BOUND('',#1083,.T.);
#446=FACE_BOUND('',#1086,.T.);
#447=FACE_BOUND('',#1089,.T.);
#448=FACE_BOUND('',#1104,.T.);
#449=FACE_BOUND('',#1109,.T.);
#450=FACE_BOUND('',#1112,.T.);
#451=FACE_BOUND('',#1120,.T.);
#452=FACE_BOUND('',#1121,.T.);
#453=FACE_BOUND('',#1123,.T.);
#454=FACE_BOUND('',#1124,.T.);
#455=FACE_BOUND('',#1140,.T.);
#456=FACE_BOUND('',#1142,.T.);
#457=FACE_BOUND('',#1148,.T.);
#458=FACE_BOUND('',#1149,.T.);
#459=FACE_BOUND('',#1150,.T.);
#460=FACE_BOUND('',#1151,.T.);
#461=FACE_BOUND('',#1152,.T.);
#462=FACE_BOUND('',#1154,.T.);
#463=FACE_BOUND('',#1155,.T.);
#464=FACE_BOUND('',#1156,.T.);
#465=FACE_BOUND('',#1157,.T.);
#466=FACE_BOUND('',#1172,.T.);
#467=FACE_BOUND('',#1187,.T.);
#468=FACE_BOUND('',#1198,.T.);
#469=FACE_BOUND('',#1200,.T.);
#470=FACE_BOUND('',#1208,.T.);
#471=FACE_BOUND('',#1210,.T.);
#472=FACE_BOUND('',#1212,.T.);
#473=FACE_BOUND('',#1214,.T.);
#474=FACE_BOUND('',#1223,.T.);
#475=FACE_BOUND('',#1244,.T.);
#476=FACE_BOUND('',#1245,.T.);
#477=FACE_BOUND('',#1246,.T.);
#478=FACE_BOUND('',#1247,.T.);
#479=FACE_BOUND('',#1248,.T.);
#480=FACE_BOUND('',#1249,.T.);
#481=FACE_BOUND('',#1252,.T.);
#482=FACE_BOUND('',#1253,.T.);
#483=FACE_BOUND('',#1254,.T.);
#484=FACE_BOUND('',#1255,.T.);
#485=FACE_BOUND('',#1256,.T.);
#486=FACE_BOUND('',#1257,.T.);
#487=FACE_BOUND('',#1259,.T.);
#488=FACE_BOUND('',#1260,.T.);
#489=FACE_BOUND('',#1261,.T.);
#490=FACE_BOUND('',#1262,.T.);
#491=FACE_BOUND('',#1274,.T.);
#492=FACE_BOUND('',#1275,.T.);
#493=FACE_BOUND('',#1276,.T.);
#494=FACE_BOUND('',#1277,.T.);
#495=FACE_BOUND('',#1278,.T.);
#496=FACE_BOUND('',#1280,.T.);
#497=FACE_BOUND('',#1281,.T.);
#498=FACE_BOUND('',#1282,.T.);
#499=FACE_BOUND('',#1283,.T.);
#500=FACE_BOUND('',#1284,.T.);
#501=FACE_BOUND('',#1291,.T.);
#502=FACE_BOUND('',#1294,.T.);
#503=FACE_BOUND('',#1297,.T.);
#504=FACE_BOUND('',#1300,.T.);
#505=FACE_BOUND('',#1303,.T.);
#506=FACE_BOUND('',#1306,.T.);
#507=FACE_BOUND('',#1308,.T.);
#508=FACE_BOUND('',#1314,.T.);
#509=FACE_BOUND('',#1316,.T.);
#510=FACE_BOUND('',#1318,.T.);
#511=FACE_BOUND('',#1320,.T.);
#512=FACE_BOUND('',#1329,.T.);
#513=FACE_BOUND('',#1330,.T.);
#514=FACE_BOUND('',#1331,.T.);
#515=FACE_BOUND('',#1332,.T.);
#516=FACE_BOUND('',#1333,.T.);
#517=FACE_BOUND('',#1334,.T.);
#518=FACE_BOUND('',#1337,.T.);
#519=FACE_BOUND('',#1338,.T.);
#520=FACE_BOUND('',#1339,.T.);
#521=FACE_BOUND('',#1340,.T.);
#522=FACE_BOUND('',#1341,.T.);
#523=FACE_BOUND('',#1342,.T.);
#524=FACE_BOUND('',#1350,.T.);
#525=FACE_BOUND('',#1368,.T.);
#526=FACE_BOUND('',#1384,.T.);
#527=FACE_BOUND('',#1386,.T.);
#528=FACE_BOUND('',#1390,.T.);
#529=FACE_BOUND('',#1392,.T.);
#530=FACE_BOUND('',#1398,.T.);
#531=PLANE('',#5340);
#532=PLANE('',#5341);
#533=PLANE('',#5342);
#534=PLANE('',#5343);
#535=PLANE('',#5344);
#536=PLANE('',#5345);
#537=PLANE('',#5352);
#538=PLANE('',#5355);
#539=PLANE('',#5357);
#540=PLANE('',#5364);
#541=PLANE('',#5365);
#542=PLANE('',#5367);
#543=PLANE('',#5369);
#544=PLANE('',#5383);
#545=PLANE('',#5384);
#546=PLANE('',#5385);
#547=PLANE('',#5386);
#548=PLANE('',#5387);
#549=PLANE('',#5388);
#550=PLANE('',#5389);
#551=PLANE('',#5390);
#552=PLANE('',#5391);
#553=PLANE('',#5392);
#554=PLANE('',#5393);
#555=PLANE('',#5395);
#556=PLANE('',#5396);
#557=PLANE('',#5397);
#558=PLANE('',#5398);
#559=PLANE('',#5399);
#560=PLANE('',#5400);
#561=PLANE('',#5401);
#562=PLANE('',#5402);
#563=PLANE('',#5403);
#564=PLANE('',#5405);
#565=PLANE('',#5413);
#566=PLANE('',#5422);
#567=PLANE('',#5427);
#568=PLANE('',#5433);
#569=PLANE('',#5434);
#570=PLANE('',#5435);
#571=PLANE('',#5436);
#572=PLANE('',#5437);
#573=PLANE('',#5438);
#574=PLANE('',#5440);
#575=PLANE('',#5441);
#576=PLANE('',#5442);
#577=PLANE('',#5443);
#578=PLANE('',#5444);
#579=PLANE('',#5445);
#580=PLANE('',#5462);
#581=PLANE('',#5463);
#582=PLANE('',#5464);
#583=PLANE('',#5465);
#584=PLANE('',#5466);
#585=PLANE('',#5467);
#586=PLANE('',#5468);
#587=PLANE('',#5469);
#588=PLANE('',#5470);
#589=PLANE('',#5471);
#590=PLANE('',#5472);
#591=PLANE('',#5474);
#592=PLANE('',#5475);
#593=PLANE('',#5476);
#594=PLANE('',#5477);
#595=PLANE('',#5478);
#596=PLANE('',#5479);
#597=PLANE('',#5480);
#598=PLANE('',#5481);
#599=PLANE('',#5482);
#600=PLANE('',#5484);
#601=PLANE('',#5492);
#602=PLANE('',#5503);
#603=PLANE('',#5506);
#604=PLANE('',#5507);
#605=PLANE('',#5508);
#606=PLANE('',#5509);
#607=PLANE('',#5510);
#608=PLANE('',#5511);
#609=PLANE('',#5512);
#610=PLANE('',#5513);
#611=PLANE('',#5519);
#612=PLANE('',#5520);
#613=PLANE('',#5521);
#614=PLANE('',#5525);
#615=PLANE('',#5526);
#616=PLANE('',#5527);
#617=PLANE('',#5528);
#618=PLANE('',#5529);
#619=PLANE('',#5533);
#620=PLANE('',#5534);
#621=PLANE('',#5536);
#622=PLANE('',#5541);
#623=PLANE('',#5548);
#624=PLANE('',#5549);
#625=PLANE('',#5551);
#626=PLANE('',#5552);
#627=PLANE('',#5553);
#628=PLANE('',#5554);
#629=PLANE('',#5555);
#630=PLANE('',#5556);
#631=PLANE('',#5557);
#632=PLANE('',#5558);
#633=PLANE('',#5566);
#634=PLANE('',#5584);
#635=PLANE('',#5588);
#636=PLANE('',#5592);
#637=PLANE('',#5596);
#638=PLANE('',#5603);
#639=PLANE('',#5604);
#640=PLANE('',#5605);
#641=PLANE('',#5606);
#642=PLANE('',#5607);
#643=PLANE('',#5608);
#644=PLANE('',#5625);
#645=PLANE('',#5626);
#646=PLANE('',#5627);
#647=PLANE('',#5628);
#648=PLANE('',#5629);
#649=PLANE('',#5630);
#650=PLANE('',#5633);
#651=PLANE('',#5635);
#652=PLANE('',#5636);
#653=PLANE('',#5638);
#654=PLANE('',#5639);
#655=PLANE('',#5640);
#656=PLANE('',#5645);
#657=PLANE('',#5649);
#658=PLANE('',#5653);
#659=PLANE('',#5657);
#660=PLANE('',#5661);
#661=PLANE('',#5665);
#662=PLANE('',#5668);
#663=PLANE('',#5669);
#664=PLANE('',#5672);
#665=PLANE('',#5673);
#666=PLANE('',#5678);
#667=PLANE('',#5702);
#668=PLANE('',#5703);
#669=PLANE('',#5704);
#670=PLANE('',#5705);
#671=PLANE('',#5706);
#672=PLANE('',#5707);
#673=PLANE('',#5709);
#674=PLANE('',#5717);
#675=PLANE('',#5725);
#676=PLANE('',#5726);
#677=PLANE('',#5727);
#678=PLANE('',#5728);
#679=PLANE('',#5729);
#680=PLANE('',#5730);
#681=PLANE('',#5731);
#682=PLANE('',#5732);
#683=PLANE('',#5733);
#684=PLANE('',#5735);
#685=PLANE('',#5743);
#686=PLANE('',#5751);
#687=PLANE('',#5752);
#688=PLANE('',#5753);
#689=PLANE('',#5754);
#690=PLANE('',#5755);
#691=PLANE('',#5756);
#692=PLANE('',#5757);
#693=PLANE('',#5758);
#694=PLANE('',#5759);
#695=PLANE('',#5804);
#696=PLANE('',#5805);
#697=PLANE('',#5813);
#698=PLANE('',#5814);
#699=PLANE('',#5816);
#700=PLANE('',#5824);
#701=PLANE('',#5832);
#702=PLANE('',#5833);
#703=PLANE('',#5834);
#704=PLANE('',#5835);
#705=PLANE('',#5836);
#706=PLANE('',#5837);
#707=PLANE('',#5838);
#708=PLANE('',#5839);
#709=PLANE('',#5840);
#710=FACE_OUTER_BOUND('',#998,.T.);
#711=FACE_OUTER_BOUND('',#999,.T.);
#712=FACE_OUTER_BOUND('',#1000,.T.);
#713=FACE_OUTER_BOUND('',#1001,.T.);
#714=FACE_OUTER_BOUND('',#1002,.T.);
#715=FACE_OUTER_BOUND('',#1003,.T.);
#716=FACE_OUTER_BOUND('',#1004,.T.);
#717=FACE_OUTER_BOUND('',#1005,.T.);
#718=FACE_OUTER_BOUND('',#1006,.T.);
#719=FACE_OUTER_BOUND('',#1007,.T.);
#720=FACE_OUTER_BOUND('',#1008,.T.);
#721=FACE_OUTER_BOUND('',#1009,.T.);
#722=FACE_OUTER_BOUND('',#1010,.T.);
#723=FACE_OUTER_BOUND('',#1011,.T.);
#724=FACE_OUTER_BOUND('',#1012,.T.);
#725=FACE_OUTER_BOUND('',#1013,.T.);
#726=FACE_OUTER_BOUND('',#1014,.T.);
#727=FACE_OUTER_BOUND('',#1015,.T.);
#728=FACE_OUTER_BOUND('',#1016,.T.);
#729=FACE_OUTER_BOUND('',#1017,.T.);
#730=FACE_OUTER_BOUND('',#1018,.T.);
#731=FACE_OUTER_BOUND('',#1035,.T.);
#732=FACE_OUTER_BOUND('',#1052,.T.);
#733=FACE_OUTER_BOUND('',#1053,.T.);
#734=FACE_OUTER_BOUND('',#1054,.T.);
#735=FACE_OUTER_BOUND('',#1055,.T.);
#736=FACE_OUTER_BOUND('',#1056,.T.);
#737=FACE_OUTER_BOUND('',#1057,.T.);
#738=FACE_OUTER_BOUND('',#1058,.T.);
#739=FACE_OUTER_BOUND('',#1059,.T.);
#740=FACE_OUTER_BOUND('',#1060,.T.);
#741=FACE_OUTER_BOUND('',#1061,.T.);
#742=FACE_OUTER_BOUND('',#1063,.T.);
#743=FACE_OUTER_BOUND('',#1065,.T.);
#744=FACE_OUTER_BOUND('',#1067,.T.);
#745=FACE_OUTER_BOUND('',#1068,.T.);
#746=FACE_OUTER_BOUND('',#1069,.T.);
#747=FACE_OUTER_BOUND('',#1070,.T.);
#748=FACE_OUTER_BOUND('',#1071,.T.);
#749=FACE_OUTER_BOUND('',#1072,.T.);
#750=FACE_OUTER_BOUND('',#1074,.T.);
#751=FACE_OUTER_BOUND('',#1075,.T.);
#752=FACE_OUTER_BOUND('',#1078,.T.);
#753=FACE_OUTER_BOUND('',#1079,.T.);
#754=FACE_OUTER_BOUND('',#1081,.T.);
#755=FACE_OUTER_BOUND('',#1082,.T.);
#756=FACE_OUTER_BOUND('',#1084,.T.);
#757=FACE_OUTER_BOUND('',#1085,.T.);
#758=FACE_OUTER_BOUND('',#1087,.T.);
#759=FACE_OUTER_BOUND('',#1088,.T.);
#760=FACE_OUTER_BOUND('',#1090,.T.);
#761=FACE_OUTER_BOUND('',#1091,.T.);
#762=FACE_OUTER_BOUND('',#1092,.T.);
#763=FACE_OUTER_BOUND('',#1093,.T.);
#764=FACE_OUTER_BOUND('',#1094,.T.);
#765=FACE_OUTER_BOUND('',#1095,.T.);
#766=FACE_OUTER_BOUND('',#1096,.T.);
#767=FACE_OUTER_BOUND('',#1097,.T.);
#768=FACE_OUTER_BOUND('',#1098,.T.);
#769=FACE_OUTER_BOUND('',#1099,.T.);
#770=FACE_OUTER_BOUND('',#1100,.T.);
#771=FACE_OUTER_BOUND('',#1101,.T.);
#772=FACE_OUTER_BOUND('',#1102,.T.);
#773=FACE_OUTER_BOUND('',#1103,.T.);
#774=FACE_OUTER_BOUND('',#1105,.T.);
#775=FACE_OUTER_BOUND('',#1106,.T.);
#776=FACE_OUTER_BOUND('',#1107,.T.);
#777=FACE_OUTER_BOUND('',#1108,.T.);
#778=FACE_OUTER_BOUND('',#1110,.T.);
#779=FACE_OUTER_BOUND('',#1111,.T.);
#780=FACE_OUTER_BOUND('',#1113,.T.);
#781=FACE_OUTER_BOUND('',#1114,.T.);
#782=FACE_OUTER_BOUND('',#1115,.T.);
#783=FACE_OUTER_BOUND('',#1116,.T.);
#784=FACE_OUTER_BOUND('',#1117,.T.);
#785=FACE_OUTER_BOUND('',#1118,.T.);
#786=FACE_OUTER_BOUND('',#1119,.T.);
#787=FACE_OUTER_BOUND('',#1122,.T.);
#788=FACE_OUTER_BOUND('',#1125,.T.);
#789=FACE_OUTER_BOUND('',#1126,.T.);
#790=FACE_OUTER_BOUND('',#1127,.T.);
#791=FACE_OUTER_BOUND('',#1128,.T.);
#792=FACE_OUTER_BOUND('',#1129,.T.);
#793=FACE_OUTER_BOUND('',#1130,.T.);
#794=FACE_OUTER_BOUND('',#1131,.T.);
#795=FACE_OUTER_BOUND('',#1132,.T.);
#796=FACE_OUTER_BOUND('',#1133,.T.);
#797=FACE_OUTER_BOUND('',#1134,.T.);
#798=FACE_OUTER_BOUND('',#1135,.T.);
#799=FACE_OUTER_BOUND('',#1136,.T.);
#800=FACE_OUTER_BOUND('',#1137,.T.);
#801=FACE_OUTER_BOUND('',#1138,.T.);
#802=FACE_OUTER_BOUND('',#1139,.T.);
#803=FACE_OUTER_BOUND('',#1141,.T.);
#804=FACE_OUTER_BOUND('',#1143,.T.);
#805=FACE_OUTER_BOUND('',#1144,.T.);
#806=FACE_OUTER_BOUND('',#1145,.T.);
#807=FACE_OUTER_BOUND('',#1146,.T.);
#808=FACE_OUTER_BOUND('',#1147,.T.);
#809=FACE_OUTER_BOUND('',#1153,.T.);
#810=FACE_OUTER_BOUND('',#1158,.T.);
#811=FACE_OUTER_BOUND('',#1159,.T.);
#812=FACE_OUTER_BOUND('',#1160,.T.);
#813=FACE_OUTER_BOUND('',#1161,.T.);
#814=FACE_OUTER_BOUND('',#1162,.T.);
#815=FACE_OUTER_BOUND('',#1163,.T.);
#816=FACE_OUTER_BOUND('',#1164,.T.);
#817=FACE_OUTER_BOUND('',#1165,.T.);
#818=FACE_OUTER_BOUND('',#1166,.T.);
#819=FACE_OUTER_BOUND('',#1167,.T.);
#820=FACE_OUTER_BOUND('',#1168,.T.);
#821=FACE_OUTER_BOUND('',#1169,.T.);
#822=FACE_OUTER_BOUND('',#1170,.T.);
#823=FACE_OUTER_BOUND('',#1171,.T.);
#824=FACE_OUTER_BOUND('',#1173,.T.);
#825=FACE_OUTER_BOUND('',#1174,.T.);
#826=FACE_OUTER_BOUND('',#1175,.T.);
#827=FACE_OUTER_BOUND('',#1176,.T.);
#828=FACE_OUTER_BOUND('',#1177,.T.);
#829=FACE_OUTER_BOUND('',#1178,.T.);
#830=FACE_OUTER_BOUND('',#1179,.T.);
#831=FACE_OUTER_BOUND('',#1180,.T.);
#832=FACE_OUTER_BOUND('',#1181,.T.);
#833=FACE_OUTER_BOUND('',#1182,.T.);
#834=FACE_OUTER_BOUND('',#1183,.T.);
#835=FACE_OUTER_BOUND('',#1184,.T.);
#836=FACE_OUTER_BOUND('',#1185,.T.);
#837=FACE_OUTER_BOUND('',#1186,.T.);
#838=FACE_OUTER_BOUND('',#1188,.T.);
#839=FACE_OUTER_BOUND('',#1189,.T.);
#840=FACE_OUTER_BOUND('',#1190,.T.);
#841=FACE_OUTER_BOUND('',#1191,.T.);
#842=FACE_OUTER_BOUND('',#1192,.T.);
#843=FACE_OUTER_BOUND('',#1193,.T.);
#844=FACE_OUTER_BOUND('',#1194,.T.);
#845=FACE_OUTER_BOUND('',#1195,.T.);
#846=FACE_OUTER_BOUND('',#1196,.T.);
#847=FACE_OUTER_BOUND('',#1197,.T.);
#848=FACE_OUTER_BOUND('',#1199,.T.);
#849=FACE_OUTER_BOUND('',#1201,.T.);
#850=FACE_OUTER_BOUND('',#1202,.T.);
#851=FACE_OUTER_BOUND('',#1203,.T.);
#852=FACE_OUTER_BOUND('',#1204,.T.);
#853=FACE_OUTER_BOUND('',#1205,.T.);
#854=FACE_OUTER_BOUND('',#1206,.T.);
#855=FACE_OUTER_BOUND('',#1207,.T.);
#856=FACE_OUTER_BOUND('',#1209,.T.);
#857=FACE_OUTER_BOUND('',#1211,.T.);
#858=FACE_OUTER_BOUND('',#1213,.T.);
#859=FACE_OUTER_BOUND('',#1215,.T.);
#860=FACE_OUTER_BOUND('',#1216,.T.);
#861=FACE_OUTER_BOUND('',#1217,.T.);
#862=FACE_OUTER_BOUND('',#1218,.T.);
#863=FACE_OUTER_BOUND('',#1219,.T.);
#864=FACE_OUTER_BOUND('',#1220,.T.);
#865=FACE_OUTER_BOUND('',#1221,.T.);
#866=FACE_OUTER_BOUND('',#1222,.T.);
#867=FACE_OUTER_BOUND('',#1224,.T.);
#868=FACE_OUTER_BOUND('',#1225,.T.);
#869=FACE_OUTER_BOUND('',#1226,.T.);
#870=FACE_OUTER_BOUND('',#1227,.T.);
#871=FACE_OUTER_BOUND('',#1228,.T.);
#872=FACE_OUTER_BOUND('',#1229,.T.);
#873=FACE_OUTER_BOUND('',#1230,.T.);
#874=FACE_OUTER_BOUND('',#1231,.T.);
#875=FACE_OUTER_BOUND('',#1232,.T.);
#876=FACE_OUTER_BOUND('',#1233,.T.);
#877=FACE_OUTER_BOUND('',#1234,.T.);
#878=FACE_OUTER_BOUND('',#1235,.T.);
#879=FACE_OUTER_BOUND('',#1236,.T.);
#880=FACE_OUTER_BOUND('',#1237,.T.);
#881=FACE_OUTER_BOUND('',#1238,.T.);
#882=FACE_OUTER_BOUND('',#1239,.T.);
#883=FACE_OUTER_BOUND('',#1240,.T.);
#884=FACE_OUTER_BOUND('',#1241,.T.);
#885=FACE_OUTER_BOUND('',#1242,.T.);
#886=FACE_OUTER_BOUND('',#1243,.T.);
#887=FACE_OUTER_BOUND('',#1250,.T.);
#888=FACE_OUTER_BOUND('',#1251,.T.);
#889=FACE_OUTER_BOUND('',#1258,.T.);
#890=FACE_OUTER_BOUND('',#1263,.T.);
#891=FACE_OUTER_BOUND('',#1264,.T.);
#892=FACE_OUTER_BOUND('',#1265,.T.);
#893=FACE_OUTER_BOUND('',#1266,.T.);
#894=FACE_OUTER_BOUND('',#1267,.T.);
#895=FACE_OUTER_BOUND('',#1268,.T.);
#896=FACE_OUTER_BOUND('',#1269,.T.);
#897=FACE_OUTER_BOUND('',#1270,.T.);
#898=FACE_OUTER_BOUND('',#1271,.T.);
#899=FACE_OUTER_BOUND('',#1272,.T.);
#900=FACE_OUTER_BOUND('',#1273,.T.);
#901=FACE_OUTER_BOUND('',#1279,.T.);
#902=FACE_OUTER_BOUND('',#1285,.T.);
#903=FACE_OUTER_BOUND('',#1286,.T.);
#904=FACE_OUTER_BOUND('',#1287,.T.);
#905=FACE_OUTER_BOUND('',#1288,.T.);
#906=FACE_OUTER_BOUND('',#1289,.T.);
#907=FACE_OUTER_BOUND('',#1290,.T.);
#908=FACE_OUTER_BOUND('',#1292,.T.);
#909=FACE_OUTER_BOUND('',#1293,.T.);
#910=FACE_OUTER_BOUND('',#1295,.T.);
#911=FACE_OUTER_BOUND('',#1296,.T.);
#912=FACE_OUTER_BOUND('',#1298,.T.);
#913=FACE_OUTER_BOUND('',#1299,.T.);
#914=FACE_OUTER_BOUND('',#1301,.T.);
#915=FACE_OUTER_BOUND('',#1302,.T.);
#916=FACE_OUTER_BOUND('',#1304,.T.);
#917=FACE_OUTER_BOUND('',#1305,.T.);
#918=FACE_OUTER_BOUND('',#1307,.T.);
#919=FACE_OUTER_BOUND('',#1309,.T.);
#920=FACE_OUTER_BOUND('',#1310,.T.);
#921=FACE_OUTER_BOUND('',#1311,.T.);
#922=FACE_OUTER_BOUND('',#1312,.T.);
#923=FACE_OUTER_BOUND('',#1313,.T.);
#924=FACE_OUTER_BOUND('',#1315,.T.);
#925=FACE_OUTER_BOUND('',#1317,.T.);
#926=FACE_OUTER_BOUND('',#1319,.T.);
#927=FACE_OUTER_BOUND('',#1321,.T.);
#928=FACE_OUTER_BOUND('',#1322,.T.);
#929=FACE_OUTER_BOUND('',#1323,.T.);
#930=FACE_OUTER_BOUND('',#1324,.T.);
#931=FACE_OUTER_BOUND('',#1325,.T.);
#932=FACE_OUTER_BOUND('',#1326,.T.);
#933=FACE_OUTER_BOUND('',#1327,.T.);
#934=FACE_OUTER_BOUND('',#1328,.T.);
#935=FACE_OUTER_BOUND('',#1335,.T.);
#936=FACE_OUTER_BOUND('',#1336,.T.);
#937=FACE_OUTER_BOUND('',#1343,.T.);
#938=FACE_OUTER_BOUND('',#1344,.T.);
#939=FACE_OUTER_BOUND('',#1345,.T.);
#940=FACE_OUTER_BOUND('',#1346,.T.);
#941=FACE_OUTER_BOUND('',#1347,.T.);
#942=FACE_OUTER_BOUND('',#1348,.T.);
#943=FACE_OUTER_BOUND('',#1349,.T.);
#944=FACE_OUTER_BOUND('',#1351,.T.);
#945=FACE_OUTER_BOUND('',#1352,.T.);
#946=FACE_OUTER_BOUND('',#1353,.T.);
#947=FACE_OUTER_BOUND('',#1354,.T.);
#948=FACE_OUTER_BOUND('',#1355,.T.);
#949=FACE_OUTER_BOUND('',#1356,.T.);
#950=FACE_OUTER_BOUND('',#1357,.T.);
#951=FACE_OUTER_BOUND('',#1358,.T.);
#952=FACE_OUTER_BOUND('',#1359,.T.);
#953=FACE_OUTER_BOUND('',#1360,.T.);
#954=FACE_OUTER_BOUND('',#1361,.T.);
#955=FACE_OUTER_BOUND('',#1362,.T.);
#956=FACE_OUTER_BOUND('',#1363,.T.);
#957=FACE_OUTER_BOUND('',#1364,.T.);
#958=FACE_OUTER_BOUND('',#1365,.T.);
#959=FACE_OUTER_BOUND('',#1366,.T.);
#960=FACE_OUTER_BOUND('',#1367,.T.);
#961=FACE_OUTER_BOUND('',#1369,.T.);
#962=FACE_OUTER_BOUND('',#1370,.T.);
#963=FACE_OUTER_BOUND('',#1371,.T.);
#964=FACE_OUTER_BOUND('',#1372,.T.);
#965=FACE_OUTER_BOUND('',#1373,.T.);
#966=FACE_OUTER_BOUND('',#1374,.T.);
#967=FACE_OUTER_BOUND('',#1375,.T.);
#968=FACE_OUTER_BOUND('',#1376,.T.);
#969=FACE_OUTER_BOUND('',#1377,.T.);
#970=FACE_OUTER_BOUND('',#1378,.T.);
#971=FACE_OUTER_BOUND('',#1379,.T.);
#972=FACE_OUTER_BOUND('',#1380,.T.);
#973=FACE_OUTER_BOUND('',#1381,.T.);
#974=FACE_OUTER_BOUND('',#1382,.T.);
#975=FACE_OUTER_BOUND('',#1383,.T.);
#976=FACE_OUTER_BOUND('',#1385,.T.);
#977=FACE_OUTER_BOUND('',#1387,.T.);
#978=FACE_OUTER_BOUND('',#1388,.T.);
#979=FACE_OUTER_BOUND('',#1389,.T.);
#980=FACE_OUTER_BOUND('',#1391,.T.);
#981=FACE_OUTER_BOUND('',#1393,.T.);
#982=FACE_OUTER_BOUND('',#1394,.T.);
#983=FACE_OUTER_BOUND('',#1395,.T.);
#984=FACE_OUTER_BOUND('',#1396,.T.);
#985=FACE_OUTER_BOUND('',#1397,.T.);
#986=FACE_OUTER_BOUND('',#1399,.T.);
#987=FACE_OUTER_BOUND('',#1400,.T.);
#988=FACE_OUTER_BOUND('',#1401,.T.);
#989=FACE_OUTER_BOUND('',#1402,.T.);
#990=FACE_OUTER_BOUND('',#1403,.T.);
#991=FACE_OUTER_BOUND('',#1404,.T.);
#992=FACE_OUTER_BOUND('',#1405,.T.);
#993=FACE_OUTER_BOUND('',#1406,.T.);
#994=FACE_OUTER_BOUND('',#1407,.T.);
#995=FACE_OUTER_BOUND('',#1408,.T.);
#996=FACE_OUTER_BOUND('',#1409,.T.);
#997=FACE_OUTER_BOUND('',#1410,.T.);
#998=EDGE_LOOP('',(#3409,#3410,#3411,#3412));
#999=EDGE_LOOP('',(#3413,#3414,#3415,#3416));
#1000=EDGE_LOOP('',(#3417,#3418,#3419,#3420));
#1001=EDGE_LOOP('',(#3421,#3422,#3423,#3424));
#1002=EDGE_LOOP('',(#3425,#3426,#3427,#3428));
#1003=EDGE_LOOP('',(#3429,#3430,#3431,#3432));
#1004=EDGE_LOOP('',(#3433,#3434,#3435,#3436));
#1005=EDGE_LOOP('',(#3437,#3438,#3439,#3440));
#1006=EDGE_LOOP('',(#3441,#3442,#3443,#3444));
#1007=EDGE_LOOP('',(#3445,#3446,#3447,#3448));
#1008=EDGE_LOOP('',(#3449,#3450,#3451,#3452));
#1009=EDGE_LOOP('',(#3453,#3454,#3455,#3456));
#1010=EDGE_LOOP('',(#3457,#3458,#3459,#3460));
#1011=EDGE_LOOP('',(#3461,#3462,#3463,#3464));
#1012=EDGE_LOOP('',(#3465,#3466,#3467,#3468));
#1013=EDGE_LOOP('',(#3469,#3470,#3471,#3472));
#1014=EDGE_LOOP('',(#3473,#3474,#3475,#3476));
#1015=EDGE_LOOP('',(#3477,#3478,#3479,#3480));
#1016=EDGE_LOOP('',(#3481,#3482,#3483,#3484));
#1017=EDGE_LOOP('',(#3485,#3486,#3487,#3488));
#1018=EDGE_LOOP('',(#3489,#3490,#3491,#3492));
#1019=EDGE_LOOP('',(#3493));
#1020=EDGE_LOOP('',(#3494));
#1021=EDGE_LOOP('',(#3495));
#1022=EDGE_LOOP('',(#3496));
#1023=EDGE_LOOP('',(#3497));
#1024=EDGE_LOOP('',(#3498));
#1025=EDGE_LOOP('',(#3499));
#1026=EDGE_LOOP('',(#3500));
#1027=EDGE_LOOP('',(#3501));
#1028=EDGE_LOOP('',(#3502));
#1029=EDGE_LOOP('',(#3503));
#1030=EDGE_LOOP('',(#3504));
#1031=EDGE_LOOP('',(#3505));
#1032=EDGE_LOOP('',(#3506));
#1033=EDGE_LOOP('',(#3507));
#1034=EDGE_LOOP('',(#3508));
#1035=EDGE_LOOP('',(#3509,#3510,#3511,#3512));
#1036=EDGE_LOOP('',(#3513));
#1037=EDGE_LOOP('',(#3514));
#1038=EDGE_LOOP('',(#3515));
#1039=EDGE_LOOP('',(#3516));
#1040=EDGE_LOOP('',(#3517));
#1041=EDGE_LOOP('',(#3518));
#1042=EDGE_LOOP('',(#3519));
#1043=EDGE_LOOP('',(#3520));
#1044=EDGE_LOOP('',(#3521));
#1045=EDGE_LOOP('',(#3522));
#1046=EDGE_LOOP('',(#3523));
#1047=EDGE_LOOP('',(#3524));
#1048=EDGE_LOOP('',(#3525));
#1049=EDGE_LOOP('',(#3526));
#1050=EDGE_LOOP('',(#3527));
#1051=EDGE_LOOP('',(#3528));
#1052=EDGE_LOOP('',(#3529,#3530,#3531,#3532));
#1053=EDGE_LOOP('',(#3533,#3534,#3535,#3536));
#1054=EDGE_LOOP('',(#3537));
#1055=EDGE_LOOP('',(#3538,#3539,#3540,#3541));
#1056=EDGE_LOOP('',(#3542));
#1057=EDGE_LOOP('',(#3543,#3544));
#1058=EDGE_LOOP('',(#3545,#3546,#3547,#3548));
#1059=EDGE_LOOP('',(#3549,#3550,#3551,#3552));
#1060=EDGE_LOOP('',(#3553,#3554));
#1061=EDGE_LOOP('',(#3555,#3556,#3557,#3558,#3559,#3560));
#1062=EDGE_LOOP('',(#3561));
#1063=EDGE_LOOP('',(#3562,#3563,#3564,#3565,#3566,#3567,#3568,#3569));
#1064=EDGE_LOOP('',(#3570));
#1065=EDGE_LOOP('',(#3571,#3572,#3573,#3574,#3575,#3576));
#1066=EDGE_LOOP('',(#3577));
#1067=EDGE_LOOP('',(#3578,#3579,#3580,#3581));
#1068=EDGE_LOOP('',(#3582,#3583,#3584,#3585));
#1069=EDGE_LOOP('',(#3586,#3587,#3588,#3589));
#1070=EDGE_LOOP('',(#3590,#3591,#3592,#3593));
#1071=EDGE_LOOP('',(#3594,#3595,#3596,#3597));
#1072=EDGE_LOOP('',(#3598,#3599,#3600,#3601,#3602,#3603,#3604,#3605,#3606,
#3607,#3608,#3609));
#1073=EDGE_LOOP('',(#3610));
#1074=EDGE_LOOP('',(#3611,#3612,#3613,#3614));
#1075=EDGE_LOOP('',(#3615,#3616,#3617,#3618));
#1076=EDGE_LOOP('',(#3619));
#1077=EDGE_LOOP('',(#3620));
#1078=EDGE_LOOP('',(#3621,#3622,#3623,#3624));
#1079=EDGE_LOOP('',(#3625,#3626,#3627,#3628,#3629,#3630,#3631,#3632));
#1080=EDGE_LOOP('',(#3633));
#1081=EDGE_LOOP('',(#3634,#3635,#3636,#3637));
#1082=EDGE_LOOP('',(#3638,#3639,#3640,#3641));
#1083=EDGE_LOOP('',(#3642));
#1084=EDGE_LOOP('',(#3643,#3644,#3645,#3646));
#1085=EDGE_LOOP('',(#3647,#3648,#3649,#3650));
#1086=EDGE_LOOP('',(#3651));
#1087=EDGE_LOOP('',(#3652,#3653,#3654,#3655));
#1088=EDGE_LOOP('',(#3656,#3657,#3658,#3659,#3660,#3661,#3662,#3663,#3664,
#3665,#3666,#3667));
#1089=EDGE_LOOP('',(#3668));
#1090=EDGE_LOOP('',(#3669,#3670,#3671,#3672));
#1091=EDGE_LOOP('',(#3673,#3674,#3675,#3676));
#1092=EDGE_LOOP('',(#3677,#3678,#3679,#3680));
#1093=EDGE_LOOP('',(#3681,#3682,#3683,#3684));
#1094=EDGE_LOOP('',(#3685,#3686,#3687,#3688));
#1095=EDGE_LOOP('',(#3689,#3690,#3691,#3692));
#1096=EDGE_LOOP('',(#3693,#3694,#3695,#3696,#3697,#3698));
#1097=EDGE_LOOP('',(#3699,#3700,#3701,#3702,#3703,#3704));
#1098=EDGE_LOOP('',(#3705));
#1099=EDGE_LOOP('',(#3706));
#1100=EDGE_LOOP('',(#3707,#3708,#3709,#3710));
#1101=EDGE_LOOP('',(#3711,#3712,#3713,#3714));
#1102=EDGE_LOOP('',(#3715,#3716,#3717,#3718));
#1103=EDGE_LOOP('',(#3719));
#1104=EDGE_LOOP('',(#3720));
#1105=EDGE_LOOP('',(#3721,#3722,#3723,#3724));
#1106=EDGE_LOOP('',(#3725,#3726,#3727,#3728));
#1107=EDGE_LOOP('',(#3729,#3730,#3731,#3732));
#1108=EDGE_LOOP('',(#3733));
#1109=EDGE_LOOP('',(#3734));
#1110=EDGE_LOOP('',(#3735,#3736,#3737,#3738));
#1111=EDGE_LOOP('',(#3739));
#1112=EDGE_LOOP('',(#3740));
#1113=EDGE_LOOP('',(#3741,#3742,#3743,#3744));
#1114=EDGE_LOOP('',(#3745,#3746,#3747,#3748));
#1115=EDGE_LOOP('',(#3749,#3750,#3751,#3752));
#1116=EDGE_LOOP('',(#3753,#3754,#3755,#3756));
#1117=EDGE_LOOP('',(#3757,#3758,#3759,#3760));
#1118=EDGE_LOOP('',(#3761,#3762,#3763,#3764));
#1119=EDGE_LOOP('',(#3765,#3766,#3767,#3768));
#1120=EDGE_LOOP('',(#3769));
#1121=EDGE_LOOP('',(#3770));
#1122=EDGE_LOOP('',(#3771,#3772,#3773,#3774));
#1123=EDGE_LOOP('',(#3775));
#1124=EDGE_LOOP('',(#3776));
#1125=EDGE_LOOP('',(#3777,#3778,#3779,#3780));
#1126=EDGE_LOOP('',(#3781,#3782,#3783,#3784));
#1127=EDGE_LOOP('',(#3785,#3786,#3787,#3788));
#1128=EDGE_LOOP('',(#3789,#3790,#3791,#3792));
#1129=EDGE_LOOP('',(#3793,#3794,#3795,#3796));
#1130=EDGE_LOOP('',(#3797,#3798,#3799,#3800));
#1131=EDGE_LOOP('',(#3801,#3802,#3803,#3804));
#1132=EDGE_LOOP('',(#3805,#3806,#3807,#3808));
#1133=EDGE_LOOP('',(#3809,#3810,#3811,#3812));
#1134=EDGE_LOOP('',(#3813,#3814,#3815,#3816));
#1135=EDGE_LOOP('',(#3817,#3818,#3819,#3820));
#1136=EDGE_LOOP('',(#3821,#3822,#3823,#3824));
#1137=EDGE_LOOP('',(#3825,#3826,#3827,#3828));
#1138=EDGE_LOOP('',(#3829,#3830,#3831,#3832));
#1139=EDGE_LOOP('',(#3833,#3834,#3835,#3836));
#1140=EDGE_LOOP('',(#3837));
#1141=EDGE_LOOP('',(#3838,#3839,#3840,#3841));
#1142=EDGE_LOOP('',(#3842));
#1143=EDGE_LOOP('',(#3843,#3844,#3845,#3846));
#1144=EDGE_LOOP('',(#3847,#3848,#3849,#3850));
#1145=EDGE_LOOP('',(#3851,#3852,#3853,#3854));
#1146=EDGE_LOOP('',(#3855,#3856,#3857,#3858));
#1147=EDGE_LOOP('',(#3859,#3860,#3861,#3862));
#1148=EDGE_LOOP('',(#3863,#3864,#3865,#3866));
#1149=EDGE_LOOP('',(#3867));
#1150=EDGE_LOOP('',(#3868));
#1151=EDGE_LOOP('',(#3869));
#1152=EDGE_LOOP('',(#3870));
#1153=EDGE_LOOP('',(#3871,#3872,#3873,#3874));
#1154=EDGE_LOOP('',(#3875));
#1155=EDGE_LOOP('',(#3876));
#1156=EDGE_LOOP('',(#3877));
#1157=EDGE_LOOP('',(#3878));
#1158=EDGE_LOOP('',(#3879,#3880,#3881,#3882));
#1159=EDGE_LOOP('',(#3883,#3884,#3885,#3886));
#1160=EDGE_LOOP('',(#3887,#3888,#3889,#3890));
#1161=EDGE_LOOP('',(#3891,#3892,#3893,#3894));
#1162=EDGE_LOOP('',(#3895,#3896,#3897,#3898));
#1163=EDGE_LOOP('',(#3899,#3900,#3901,#3902));
#1164=EDGE_LOOP('',(#3903,#3904,#3905,#3906,#3907,#3908));
#1165=EDGE_LOOP('',(#3909,#3910,#3911,#3912,#3913,#3914));
#1166=EDGE_LOOP('',(#3915));
#1167=EDGE_LOOP('',(#3916));
#1168=EDGE_LOOP('',(#3917,#3918,#3919,#3920));
#1169=EDGE_LOOP('',(#3921,#3922,#3923,#3924));
#1170=EDGE_LOOP('',(#3925,#3926,#3927,#3928));
#1171=EDGE_LOOP('',(#3929));
#1172=EDGE_LOOP('',(#3930));
#1173=EDGE_LOOP('',(#3931,#3932,#3933,#3934));
#1174=EDGE_LOOP('',(#3935,#3936,#3937,#3938));
#1175=EDGE_LOOP('',(#3939,#3940,#3941,#3942));
#1176=EDGE_LOOP('',(#3943,#3944,#3945,#3946));
#1177=EDGE_LOOP('',(#3947));
#1178=EDGE_LOOP('',(#3948,#3949,#3950,#3951,#3952,#3953,#3954,#3955,#3956));
#1179=EDGE_LOOP('',(#3957,#3958,#3959,#3960));
#1180=EDGE_LOOP('',(#3961,#3962,#3963,#3964));
#1181=EDGE_LOOP('',(#3965,#3966,#3967,#3968));
#1182=EDGE_LOOP('',(#3969,#3970,#3971,#3972));
#1183=EDGE_LOOP('',(#3973,#3974,#3975,#3976));
#1184=EDGE_LOOP('',(#3977,#3978,#3979,#3980));
#1185=EDGE_LOOP('',(#3981));
#1186=EDGE_LOOP('',(#3982,#3983,#3984,#3985,#3986,#3987));
#1187=EDGE_LOOP('',(#3988));
#1188=EDGE_LOOP('',(#3989,#3990,#3991,#3992,#3993,#3994,#3995,#3996,#3997));
#1189=EDGE_LOOP('',(#3998,#3999,#4000,#4001,#4002,#4003,#4004,#4005,#4006));
#1190=EDGE_LOOP('',(#4007,#4008,#4009,#4010));
#1191=EDGE_LOOP('',(#4011,#4012,#4013,#4014));
#1192=EDGE_LOOP('',(#4015,#4016,#4017,#4018));
#1193=EDGE_LOOP('',(#4019,#4020,#4021,#4022));
#1194=EDGE_LOOP('',(#4023,#4024,#4025,#4026));
#1195=EDGE_LOOP('',(#4027,#4028,#4029,#4030));
#1196=EDGE_LOOP('',(#4031,#4032,#4033,#4034));
#1197=EDGE_LOOP('',(#4035));
#1198=EDGE_LOOP('',(#4036));
#1199=EDGE_LOOP('',(#4037));
#1200=EDGE_LOOP('',(#4038));
#1201=EDGE_LOOP('',(#4039,#4040,#4041,#4042));
#1202=EDGE_LOOP('',(#4043));
#1203=EDGE_LOOP('',(#4044));
#1204=EDGE_LOOP('',(#4045,#4046));
#1205=EDGE_LOOP('',(#4047,#4048,#4049,#4050,#4051,#4052,#4053,#4054,#4055));
#1206=EDGE_LOOP('',(#4056,#4057,#4058));
#1207=EDGE_LOOP('',(#4059,#4060,#4061,#4062));
#1208=EDGE_LOOP('',(#4063,#4064,#4065,#4066));
#1209=EDGE_LOOP('',(#4067,#4068,#4069,#4070));
#1210=EDGE_LOOP('',(#4071,#4072));
#1211=EDGE_LOOP('',(#4073));
#1212=EDGE_LOOP('',(#4074));
#1213=EDGE_LOOP('',(#4075));
#1214=EDGE_LOOP('',(#4076));
#1215=EDGE_LOOP('',(#4077,#4078,#4079,#4080));
#1216=EDGE_LOOP('',(#4081,#4082,#4083,#4084));
#1217=EDGE_LOOP('',(#4085,#4086,#4087,#4088));
#1218=EDGE_LOOP('',(#4089,#4090,#4091,#4092));
#1219=EDGE_LOOP('',(#4093,#4094,#4095,#4096));
#1220=EDGE_LOOP('',(#4097,#4098,#4099,#4100));
#1221=EDGE_LOOP('',(#4101,#4102,#4103,#4104,#4105,#4106));
#1222=EDGE_LOOP('',(#4107));
#1223=EDGE_LOOP('',(#4108,#4109,#4110,#4111,#4112,#4113));
#1224=EDGE_LOOP('',(#4114,#4115,#4116,#4117));
#1225=EDGE_LOOP('',(#4118,#4119,#4120,#4121));
#1226=EDGE_LOOP('',(#4122,#4123,#4124,#4125));
#1227=EDGE_LOOP('',(#4126));
#1228=EDGE_LOOP('',(#4127,#4128,#4129,#4130));
#1229=EDGE_LOOP('',(#4131,#4132,#4133,#4134));
#1230=EDGE_LOOP('',(#4135,#4136,#4137,#4138));
#1231=EDGE_LOOP('',(#4139,#4140,#4141,#4142));
#1232=EDGE_LOOP('',(#4143,#4144,#4145,#4146));
#1233=EDGE_LOOP('',(#4147));
#1234=EDGE_LOOP('',(#4148,#4149,#4150,#4151));
#1235=EDGE_LOOP('',(#4152));
#1236=EDGE_LOOP('',(#4153,#4154,#4155,#4156));
#1237=EDGE_LOOP('',(#4157));
#1238=EDGE_LOOP('',(#4158,#4159,#4160,#4161));
#1239=EDGE_LOOP('',(#4162));
#1240=EDGE_LOOP('',(#4163,#4164,#4165,#4166));
#1241=EDGE_LOOP('',(#4167,#4168,#4169,#4170));
#1242=EDGE_LOOP('',(#4171,#4172,#4173,#4174));
#1243=EDGE_LOOP('',(#4175,#4176,#4177,#4178));
#1244=EDGE_LOOP('',(#4179));
#1245=EDGE_LOOP('',(#4180));
#1246=EDGE_LOOP('',(#4181));
#1247=EDGE_LOOP('',(#4182));
#1248=EDGE_LOOP('',(#4183));
#1249=EDGE_LOOP('',(#4184));
#1250=EDGE_LOOP('',(#4185,#4186,#4187,#4188));
#1251=EDGE_LOOP('',(#4189,#4190,#4191,#4192));
#1252=EDGE_LOOP('',(#4193));
#1253=EDGE_LOOP('',(#4194));
#1254=EDGE_LOOP('',(#4195));
#1255=EDGE_LOOP('',(#4196));
#1256=EDGE_LOOP('',(#4197));
#1257=EDGE_LOOP('',(#4198));
#1258=EDGE_LOOP('',(#4199,#4200,#4201,#4202));
#1259=EDGE_LOOP('',(#4203));
#1260=EDGE_LOOP('',(#4204));
#1261=EDGE_LOOP('',(#4205));
#1262=EDGE_LOOP('',(#4206));
#1263=EDGE_LOOP('',(#4207,#4208,#4209,#4210));
#1264=EDGE_LOOP('',(#4211,#4212,#4213,#4214));
#1265=EDGE_LOOP('',(#4215,#4216,#4217,#4218));
#1266=EDGE_LOOP('',(#4219,#4220,#4221,#4222));
#1267=EDGE_LOOP('',(#4223,#4224,#4225,#4226));
#1268=EDGE_LOOP('',(#4227,#4228,#4229,#4230));
#1269=EDGE_LOOP('',(#4231,#4232,#4233,#4234));
#1270=EDGE_LOOP('',(#4235,#4236,#4237,#4238));
#1271=EDGE_LOOP('',(#4239,#4240,#4241,#4242));
#1272=EDGE_LOOP('',(#4243,#4244,#4245,#4246));
#1273=EDGE_LOOP('',(#4247,#4248,#4249,#4250));
#1274=EDGE_LOOP('',(#4251));
#1275=EDGE_LOOP('',(#4252));
#1276=EDGE_LOOP('',(#4253));
#1277=EDGE_LOOP('',(#4254));
#1278=EDGE_LOOP('',(#4255));
#1279=EDGE_LOOP('',(#4256,#4257,#4258,#4259));
#1280=EDGE_LOOP('',(#4260));
#1281=EDGE_LOOP('',(#4261));
#1282=EDGE_LOOP('',(#4262));
#1283=EDGE_LOOP('',(#4263));
#1284=EDGE_LOOP('',(#4264));
#1285=EDGE_LOOP('',(#4265,#4266,#4267,#4268));
#1286=EDGE_LOOP('',(#4269,#4270,#4271,#4272));
#1287=EDGE_LOOP('',(#4273,#4274,#4275,#4276));
#1288=EDGE_LOOP('',(#4277,#4278,#4279,#4280));
#1289=EDGE_LOOP('',(#4281,#4282,#4283,#4284));
#1290=EDGE_LOOP('',(#4285));
#1291=EDGE_LOOP('',(#4286));
#1292=EDGE_LOOP('',(#4287,#4288,#4289,#4290));
#1293=EDGE_LOOP('',(#4291));
#1294=EDGE_LOOP('',(#4292));
#1295=EDGE_LOOP('',(#4293,#4294,#4295,#4296));
#1296=EDGE_LOOP('',(#4297));
#1297=EDGE_LOOP('',(#4298));
#1298=EDGE_LOOP('',(#4299,#4300,#4301,#4302));
#1299=EDGE_LOOP('',(#4303));
#1300=EDGE_LOOP('',(#4304));
#1301=EDGE_LOOP('',(#4305,#4306,#4307,#4308));
#1302=EDGE_LOOP('',(#4309));
#1303=EDGE_LOOP('',(#4310));
#1304=EDGE_LOOP('',(#4311,#4312,#4313,#4314));
#1305=EDGE_LOOP('',(#4315));
#1306=EDGE_LOOP('',(#4316));
#1307=EDGE_LOOP('',(#4317,#4318,#4319,#4320));
#1308=EDGE_LOOP('',(#4321,#4322,#4323,#4324));
#1309=EDGE_LOOP('',(#4325,#4326,#4327,#4328));
#1310=EDGE_LOOP('',(#4329,#4330,#4331,#4332));
#1311=EDGE_LOOP('',(#4333,#4334,#4335,#4336));
#1312=EDGE_LOOP('',(#4337,#4338,#4339,#4340));
#1313=EDGE_LOOP('',(#4341));
#1314=EDGE_LOOP('',(#4342));
#1315=EDGE_LOOP('',(#4343,#4344,#4345,#4346));
#1316=EDGE_LOOP('',(#4347,#4348,#4349,#4350));
#1317=EDGE_LOOP('',(#4351));
#1318=EDGE_LOOP('',(#4352));
#1319=EDGE_LOOP('',(#4353,#4354,#4355,#4356));
#1320=EDGE_LOOP('',(#4357,#4358,#4359,#4360));
#1321=EDGE_LOOP('',(#4361,#4362,#4363,#4364));
#1322=EDGE_LOOP('',(#4365,#4366,#4367,#4368));
#1323=EDGE_LOOP('',(#4369,#4370,#4371,#4372));
#1324=EDGE_LOOP('',(#4373,#4374,#4375,#4376));
#1325=EDGE_LOOP('',(#4377,#4378,#4379,#4380));
#1326=EDGE_LOOP('',(#4381,#4382,#4383,#4384));
#1327=EDGE_LOOP('',(#4385,#4386,#4387,#4388));
#1328=EDGE_LOOP('',(#4389,#4390,#4391,#4392));
#1329=EDGE_LOOP('',(#4393));
#1330=EDGE_LOOP('',(#4394));
#1331=EDGE_LOOP('',(#4395));
#1332=EDGE_LOOP('',(#4396));
#1333=EDGE_LOOP('',(#4397));
#1334=EDGE_LOOP('',(#4398));
#1335=EDGE_LOOP('',(#4399,#4400,#4401,#4402));
#1336=EDGE_LOOP('',(#4403,#4404,#4405,#4406));
#1337=EDGE_LOOP('',(#4407));
#1338=EDGE_LOOP('',(#4408));
#1339=EDGE_LOOP('',(#4409));
#1340=EDGE_LOOP('',(#4410));
#1341=EDGE_LOOP('',(#4411));
#1342=EDGE_LOOP('',(#4412));
#1343=EDGE_LOOP('',(#4413,#4414,#4415,#4416));
#1344=EDGE_LOOP('',(#4417,#4418,#4419,#4420));
#1345=EDGE_LOOP('',(#4421));
#1346=EDGE_LOOP('',(#4422,#4423,#4424,#4425));
#1347=EDGE_LOOP('',(#4426,#4427,#4428,#4429));
#1348=EDGE_LOOP('',(#4430,#4431,#4432,#4433));
#1349=EDGE_LOOP('',(#4434));
#1350=EDGE_LOOP('',(#4435));
#1351=EDGE_LOOP('',(#4436,#4437,#4438,#4439));
#1352=EDGE_LOOP('',(#4440,#4441,#4442,#4443));
#1353=EDGE_LOOP('',(#4444,#4445,#4446,#4447));
#1354=EDGE_LOOP('',(#4448));
#1355=EDGE_LOOP('',(#4449,#4450,#4451,#4452));
#1356=EDGE_LOOP('',(#4453,#4454,#4455,#4456));
#1357=EDGE_LOOP('',(#4457,#4458,#4459,#4460));
#1358=EDGE_LOOP('',(#4461,#4462,#4463,#4464));
#1359=EDGE_LOOP('',(#4465,#4466,#4467,#4468));
#1360=EDGE_LOOP('',(#4469,#4470,#4471,#4472));
#1361=EDGE_LOOP('',(#4473,#4474,#4475,#4476,#4477,#4478));
#1362=EDGE_LOOP('',(#4479,#4480,#4481,#4482,#4483,#4484));
#1363=EDGE_LOOP('',(#4485));
#1364=EDGE_LOOP('',(#4486,#4487,#4488,#4489));
#1365=EDGE_LOOP('',(#4490,#4491,#4492,#4493));
#1366=EDGE_LOOP('',(#4494,#4495,#4496,#4497));
#1367=EDGE_LOOP('',(#4498));
#1368=EDGE_LOOP('',(#4499));
#1369=EDGE_LOOP('',(#4500,#4501,#4502,#4503));
#1370=EDGE_LOOP('',(#4504,#4505,#4506,#4507));
#1371=EDGE_LOOP('',(#4508,#4509,#4510,#4511));
#1372=EDGE_LOOP('',(#4512));
#1373=EDGE_LOOP('',(#4513,#4514,#4515,#4516));
#1374=EDGE_LOOP('',(#4517,#4518,#4519,#4520));
#1375=EDGE_LOOP('',(#4521,#4522,#4523,#4524));
#1376=EDGE_LOOP('',(#4525,#4526,#4527,#4528));
#1377=EDGE_LOOP('',(#4529,#4530,#4531,#4532));
#1378=EDGE_LOOP('',(#4533,#4534,#4535,#4536));
#1379=EDGE_LOOP('',(#4537,#4538,#4539,#4540,#4541,#4542));
#1380=EDGE_LOOP('',(#4543,#4544,#4545,#4546,#4547,#4548));
#1381=EDGE_LOOP('',(#4549,#4550,#4551,#4552));
#1382=EDGE_LOOP('',(#4553,#4554,#4555,#4556));
#1383=EDGE_LOOP('',(#4557));
#1384=EDGE_LOOP('',(#4558));
#1385=EDGE_LOOP('',(#4559));
#1386=EDGE_LOOP('',(#4560));
#1387=EDGE_LOOP('',(#4561,#4562,#4563,#4564));
#1388=EDGE_LOOP('',(#4565,#4566,#4567,#4568));
#1389=EDGE_LOOP('',(#4569));
#1390=EDGE_LOOP('',(#4570));
#1391=EDGE_LOOP('',(#4571));
#1392=EDGE_LOOP('',(#4572));
#1393=EDGE_LOOP('',(#4573));
#1394=EDGE_LOOP('',(#4574,#4575,#4576,#4577));
#1395=EDGE_LOOP('',(#4578,#4579,#4580,#4581));
#1396=EDGE_LOOP('',(#4582,#4583,#4584,#4585));
#1397=EDGE_LOOP('',(#4586));
#1398=EDGE_LOOP('',(#4587));
#1399=EDGE_LOOP('',(#4588,#4589,#4590,#4591));
#1400=EDGE_LOOP('',(#4592,#4593,#4594,#4595));
#1401=EDGE_LOOP('',(#4596,#4597,#4598,#4599));
#1402=EDGE_LOOP('',(#4600));
#1403=EDGE_LOOP('',(#4601,#4602,#4603,#4604));
#1404=EDGE_LOOP('',(#4605,#4606,#4607,#4608));
#1405=EDGE_LOOP('',(#4609,#4610,#4611,#4612));
#1406=EDGE_LOOP('',(#4613,#4614,#4615,#4616));
#1407=EDGE_LOOP('',(#4617,#4618,#4619,#4620));
#1408=EDGE_LOOP('',(#4621,#4622,#4623,#4624));
#1409=EDGE_LOOP('',(#4625,#4626,#4627,#4628,#4629,#4630));
#1410=EDGE_LOOP('',(#4631,#4632,#4633,#4634,#4635,#4636));
#1411=LINE('',#7413,#1803);
#1412=LINE('',#7419,#1804);
#1413=LINE('',#7425,#1805);
#1414=LINE('',#7431,#1806);
#1415=LINE('',#7437,#1807);
#1416=LINE('',#7443,#1808);
#1417=LINE('',#7449,#1809);
#1418=LINE('',#7455,#1810);
#1419=LINE('',#7461,#1811);
#1420=LINE('',#7467,#1812);
#1421=LINE('',#7473,#1813);
#1422=LINE('',#7479,#1814);
#1423=LINE('',#7485,#1815);
#1424=LINE('',#7491,#1816);
#1425=LINE('',#7497,#1817);
#1426=LINE('',#7503,#1818);
#1427=LINE('',#7508,#1819);
#1428=LINE('',#7510,#1820);
#1429=LINE('',#7512,#1821);
#1430=LINE('',#7513,#1822);
#1431=LINE('',#7516,#1823);
#1432=LINE('',#7518,#1824);
#1433=LINE('',#7519,#1825);
#1434=LINE('',#7522,#1826);
#1435=LINE('',#7524,#1827);
#1436=LINE('',#7525,#1828);
#1437=LINE('',#7527,#1829);
#1438=LINE('',#7528,#1830);
#1439=LINE('',#7536,#1831);
#1440=LINE('',#7541,#1832);
#1441=LINE('',#7546,#1833);
#1442=LINE('',#7552,#1834);
#1443=LINE('',#7556,#1835);
#1444=LINE('',#7559,#1836);
#1445=LINE('',#7563,#1837);
#1446=LINE('',#7567,#1838);
#1447=LINE('',#7570,#1839);
#1448=LINE('',#7573,#1840);
#1449=LINE('',#7575,#1841);
#1450=LINE('',#7577,#1842);
#1451=LINE('',#7579,#1843);
#1452=LINE('',#7580,#1844);
#1453=LINE('',#7585,#1845);
#1454=LINE('',#7587,#1846);
#1455=LINE('',#7588,#1847);
#1456=LINE('',#7594,#1848);
#1457=LINE('',#7596,#1849);
#1458=LINE('',#7597,#1850);
#1459=LINE('',#7599,#1851);
#1460=LINE('',#7600,#1852);
#1461=LINE('',#7607,#1853);
#1462=LINE('',#7611,#1854);
#1463=LINE('',#7616,#1855);
#1464=LINE('',#7620,#1856);
#1465=LINE('',#7625,#1857);
#1466=LINE('',#7629,#1858);
#1467=LINE('',#7631,#1859);
#1468=LINE('',#7632,#1860);
#1469=LINE('',#7634,#1861);
#1470=LINE('',#7636,#1862);
#1471=LINE('',#7638,#1863);
#1472=LINE('',#7640,#1864);
#1473=LINE('',#7642,#1865);
#1474=LINE('',#7643,#1866);
#1475=LINE('',#7646,#1867);
#1476=LINE('',#7647,#1868);
#1477=LINE('',#7650,#1869);
#1478=LINE('',#7651,#1870);
#1479=LINE('',#7653,#1871);
#1480=LINE('',#7656,#1872);
#1481=LINE('',#7657,#1873);
#1482=LINE('',#7660,#1874);
#1483=LINE('',#7661,#1875);
#1484=LINE('',#7664,#1876);
#1485=LINE('',#7665,#1877);
#1486=LINE('',#7668,#1878);
#1487=LINE('',#7669,#1879);
#1488=LINE('',#7672,#1880);
#1489=LINE('',#7673,#1881);
#1490=LINE('',#7675,#1882);
#1491=LINE('',#7681,#1883);
#1492=LINE('',#7683,#1884);
#1493=LINE('',#7685,#1885);
#1494=LINE('',#7686,#1886);
#1495=LINE('',#7689,#1887);
#1496=LINE('',#7691,#1888);
#1497=LINE('',#7692,#1889);
#1498=LINE('',#7695,#1890);
#1499=LINE('',#7697,#1891);
#1500=LINE('',#7698,#1892);
#1501=LINE('',#7701,#1893);
#1502=LINE('',#7703,#1894);
#1503=LINE('',#7704,#1895);
#1504=LINE('',#7707,#1896);
#1505=LINE('',#7709,#1897);
#1506=LINE('',#7710,#1898);
#1507=LINE('',#7712,#1899);
#1508=LINE('',#7713,#1900);
#1509=LINE('',#7725,#1901);
#1510=LINE('',#7729,#1902);
#1511=LINE('',#7733,#1903);
#1512=LINE('',#7740,#1904);
#1513=LINE('',#7742,#1905);
#1514=LINE('',#7748,#1906);
#1515=LINE('',#7757,#1907);
#1516=LINE('',#7765,#1908);
#1517=LINE('',#7769,#1909);
#1518=LINE('',#7773,#1910);
#1519=LINE('',#7775,#1911);
#1520=LINE('',#7777,#1912);
#1521=LINE('',#7778,#1913);
#1522=LINE('',#7781,#1914);
#1523=LINE('',#7783,#1915);
#1524=LINE('',#7784,#1916);
#1525=LINE('',#7787,#1917);
#1526=LINE('',#7789,#1918);
#1527=LINE('',#7790,#1919);
#1528=LINE('',#7792,#1920);
#1529=LINE('',#7793,#1921);
#1530=LINE('',#7800,#1922);
#1531=LINE('',#7802,#1923);
#1532=LINE('',#7804,#1924);
#1533=LINE('',#7805,#1925);
#1534=LINE('',#7808,#1926);
#1535=LINE('',#7810,#1927);
#1536=LINE('',#7811,#1928);
#1537=LINE('',#7814,#1929);
#1538=LINE('',#7816,#1930);
#1539=LINE('',#7817,#1931);
#1540=LINE('',#7819,#1932);
#1541=LINE('',#7820,#1933);
#1542=LINE('',#7828,#1934);
#1543=LINE('',#7834,#1935);
#1544=LINE('',#7840,#1936);
#1545=LINE('',#7846,#1937);
#1546=LINE('',#7852,#1938);
#1547=LINE('',#7857,#1939);
#1548=LINE('',#7859,#1940);
#1549=LINE('',#7861,#1941);
#1550=LINE('',#7862,#1942);
#1551=LINE('',#7865,#1943);
#1552=LINE('',#7867,#1944);
#1553=LINE('',#7868,#1945);
#1554=LINE('',#7871,#1946);
#1555=LINE('',#7873,#1947);
#1556=LINE('',#7874,#1948);
#1557=LINE('',#7876,#1949);
#1558=LINE('',#7878,#1950);
#1559=LINE('',#7882,#1951);
#1560=LINE('',#7884,#1952);
#1561=LINE('',#7886,#1953);
#1562=LINE('',#7887,#1954);
#1563=LINE('',#7890,#1955);
#1564=LINE('',#7892,#1956);
#1565=LINE('',#7893,#1957);
#1566=LINE('',#7896,#1958);
#1567=LINE('',#7898,#1959);
#1568=LINE('',#7899,#1960);
#1569=LINE('',#7901,#1961);
#1570=LINE('',#7902,#1962);
#1571=LINE('',#7909,#1963);
#1572=LINE('',#7911,#1964);
#1573=LINE('',#7913,#1965);
#1574=LINE('',#7914,#1966);
#1575=LINE('',#7917,#1967);
#1576=LINE('',#7919,#1968);
#1577=LINE('',#7920,#1969);
#1578=LINE('',#7923,#1970);
#1579=LINE('',#7925,#1971);
#1580=LINE('',#7926,#1972);
#1581=LINE('',#7929,#1973);
#1582=LINE('',#7931,#1974);
#1583=LINE('',#7932,#1975);
#1584=LINE('',#7935,#1976);
#1585=LINE('',#7937,#1977);
#1586=LINE('',#7938,#1978);
#1587=LINE('',#7940,#1979);
#1588=LINE('',#7941,#1980);
#1589=LINE('',#7953,#1981);
#1590=LINE('',#7957,#1982);
#1591=LINE('',#7961,#1983);
#1592=LINE('',#7968,#1984);
#1593=LINE('',#7970,#1985);
#1594=LINE('',#7976,#1986);
#1595=LINE('',#7981,#1987);
#1596=LINE('',#7987,#1988);
#1597=LINE('',#8013,#1989);
#1598=LINE('',#8015,#1990);
#1599=LINE('',#8016,#1991);
#1600=LINE('',#8019,#1992);
#1601=LINE('',#8020,#1993);
#1602=LINE('',#8023,#1994);
#1603=LINE('',#8024,#1995);
#1604=LINE('',#8027,#1996);
#1605=LINE('',#8028,#1997);
#1606=LINE('',#8031,#1998);
#1607=LINE('',#8032,#1999);
#1608=LINE('',#8034,#2000);
#1609=LINE('',#8049,#2001);
#1610=LINE('',#8070,#2002);
#1611=LINE('',#8095,#2003);
#1612=LINE('',#8096,#2004);
#1613=LINE('',#8098,#2005);
#1614=LINE('',#8100,#2006);
#1615=LINE('',#8105,#2007);
#1616=LINE('',#8108,#2008);
#1617=LINE('',#8110,#2009);
#1618=LINE('',#9478,#2010);
#1619=LINE('',#9495,#2011);
#1620=LINE('',#9546,#2012);
#1621=LINE('',#9551,#2013);
#1622=LINE('',#9557,#2014);
#1623=LINE('',#9565,#2015);
#1624=LINE('',#9567,#2016);
#1625=LINE('',#9569,#2017);
#1626=LINE('',#9570,#2018);
#1627=LINE('',#9573,#2019);
#1628=LINE('',#9575,#2020);
#1629=LINE('',#9576,#2021);
#1630=LINE('',#9579,#2022);
#1631=LINE('',#9581,#2023);
#1632=LINE('',#9582,#2024);
#1633=LINE('',#9585,#2025);
#1634=LINE('',#9587,#2026);
#1635=LINE('',#9588,#2027);
#1636=LINE('',#9591,#2028);
#1637=LINE('',#9593,#2029);
#1638=LINE('',#9594,#2030);
#1639=LINE('',#9596,#2031);
#1640=LINE('',#9597,#2032);
#1641=LINE('',#9605,#2033);
#1642=LINE('',#9609,#2034);
#1643=LINE('',#9613,#2035);
#1644=LINE('',#9621,#2036);
#1645=LINE('',#9627,#2037);
#1646=LINE('',#9633,#2038);
#1647=LINE('',#9639,#2039);
#1648=LINE('',#9645,#2040);
#1649=LINE('',#9652,#2041);
#1650=LINE('',#9659,#2042);
#1651=LINE('',#9666,#2043);
#1652=LINE('',#9673,#2044);
#1653=LINE('',#9679,#2045);
#1654=LINE('',#9684,#2046);
#1655=LINE('',#9686,#2047);
#1656=LINE('',#9688,#2048);
#1657=LINE('',#9689,#2049);
#1658=LINE('',#9692,#2050);
#1659=LINE('',#9694,#2051);
#1660=LINE('',#9695,#2052);
#1661=LINE('',#9698,#2053);
#1662=LINE('',#9700,#2054);
#1663=LINE('',#9701,#2055);
#1664=LINE('',#9703,#2056);
#1665=LINE('',#9704,#2057);
#1666=LINE('',#9712,#2058);
#1667=LINE('',#9718,#2059);
#1668=LINE('',#9724,#2060);
#1669=LINE('',#9730,#2061);
#1670=LINE('',#9736,#2062);
#1671=LINE('',#9741,#2063);
#1672=LINE('',#9743,#2064);
#1673=LINE('',#9745,#2065);
#1674=LINE('',#9746,#2066);
#1675=LINE('',#9749,#2067);
#1676=LINE('',#9751,#2068);
#1677=LINE('',#9752,#2069);
#1678=LINE('',#9755,#2070);
#1679=LINE('',#9757,#2071);
#1680=LINE('',#9758,#2072);
#1681=LINE('',#9760,#2073);
#1682=LINE('',#9761,#2074);
#1683=LINE('',#9771,#2075);
#1684=LINE('',#9773,#2076);
#1685=LINE('',#9774,#2077);
#1686=LINE('',#9777,#2078);
#1687=LINE('',#9779,#2079);
#1688=LINE('',#9780,#2080);
#1689=LINE('',#9785,#2081);
#1690=LINE('',#9786,#2082);
#1691=LINE('',#9788,#2083);
#1692=LINE('',#9789,#2084);
#1693=LINE('',#9799,#2085);
#1694=LINE('',#9806,#2086);
#1695=LINE('',#9813,#2087);
#1696=LINE('',#9820,#2088);
#1697=LINE('',#9827,#2089);
#1698=LINE('',#9832,#2090);
#1699=LINE('',#9839,#2091);
#1700=LINE('',#9842,#2092);
#1701=LINE('',#9845,#2093);
#1702=LINE('',#9847,#2094);
#1703=LINE('',#9848,#2095);
#1704=LINE('',#9854,#2096);
#1705=LINE('',#9856,#2097);
#1706=LINE('',#9857,#2098);
#1707=LINE('',#9866,#2099);
#1708=LINE('',#9871,#2100);
#1709=LINE('',#9879,#2101);
#1710=LINE('',#9885,#2102);
#1711=LINE('',#9891,#2103);
#1712=LINE('',#9897,#2104);
#1713=LINE('',#9903,#2105);
#1714=LINE('',#9909,#2106);
#1715=LINE('',#9914,#2107);
#1716=LINE('',#9916,#2108);
#1717=LINE('',#9918,#2109);
#1718=LINE('',#9919,#2110);
#1719=LINE('',#9922,#2111);
#1720=LINE('',#9924,#2112);
#1721=LINE('',#9925,#2113);
#1722=LINE('',#9928,#2114);
#1723=LINE('',#9930,#2115);
#1724=LINE('',#9931,#2116);
#1725=LINE('',#9933,#2117);
#1726=LINE('',#9934,#2118);
#1727=LINE('',#9944,#2119);
#1728=LINE('',#9948,#2120);
#1729=LINE('',#9952,#2121);
#1730=LINE('',#9959,#2122);
#1731=LINE('',#9963,#2123);
#1732=LINE('',#9967,#2124);
#1733=LINE('',#9972,#2125);
#1734=LINE('',#9974,#2126);
#1735=LINE('',#9976,#2127);
#1736=LINE('',#9977,#2128);
#1737=LINE('',#9980,#2129);
#1738=LINE('',#9982,#2130);
#1739=LINE('',#9983,#2131);
#1740=LINE('',#9986,#2132);
#1741=LINE('',#9988,#2133);
#1742=LINE('',#9989,#2134);
#1743=LINE('',#9992,#2135);
#1744=LINE('',#9994,#2136);
#1745=LINE('',#9995,#2137);
#1746=LINE('',#9998,#2138);
#1747=LINE('',#10000,#2139);
#1748=LINE('',#10001,#2140);
#1749=LINE('',#10003,#2141);
#1750=LINE('',#10004,#2142);
#1751=LINE('',#10014,#2143);
#1752=LINE('',#10018,#2144);
#1753=LINE('',#10022,#2145);
#1754=LINE('',#10029,#2146);
#1755=LINE('',#10033,#2147);
#1756=LINE('',#10037,#2148);
#1757=LINE('',#10042,#2149);
#1758=LINE('',#10044,#2150);
#1759=LINE('',#10046,#2151);
#1760=LINE('',#10047,#2152);
#1761=LINE('',#10050,#2153);
#1762=LINE('',#10052,#2154);
#1763=LINE('',#10053,#2155);
#1764=LINE('',#10056,#2156);
#1765=LINE('',#10058,#2157);
#1766=LINE('',#10059,#2158);
#1767=LINE('',#10062,#2159);
#1768=LINE('',#10064,#2160);
#1769=LINE('',#10065,#2161);
#1770=LINE('',#10068,#2162);
#1771=LINE('',#10070,#2163);
#1772=LINE('',#10071,#2164);
#1773=LINE('',#10073,#2165);
#1774=LINE('',#10074,#2166);
#1775=LINE('',#10119,#2167);
#1776=LINE('',#10125,#2168);
#1777=LINE('',#10134,#2169);
#1778=LINE('',#10140,#2170);
#1779=LINE('',#10151,#2171);
#1780=LINE('',#10155,#2172);
#1781=LINE('',#10159,#2173);
#1782=LINE('',#10166,#2174);
#1783=LINE('',#10170,#2175);
#1784=LINE('',#10174,#2176);
#1785=LINE('',#10179,#2177);
#1786=LINE('',#10181,#2178);
#1787=LINE('',#10183,#2179);
#1788=LINE('',#10184,#2180);
#1789=LINE('',#10187,#2181);
#1790=LINE('',#10189,#2182);
#1791=LINE('',#10190,#2183);
#1792=LINE('',#10193,#2184);
#1793=LINE('',#10195,#2185);
#1794=LINE('',#10196,#2186);
#1795=LINE('',#10199,#2187);
#1796=LINE('',#10201,#2188);
#1797=LINE('',#10202,#2189);
#1798=LINE('',#10205,#2190);
#1799=LINE('',#10207,#2191);
#1800=LINE('',#10208,#2192);
#1801=LINE('',#10210,#2193);
#1802=LINE('',#10211,#2194);
#1803=VECTOR('',#5874,0.210000000000001);
#1804=VECTOR('',#5881,0.210000000000001);
#1805=VECTOR('',#5888,0.210000000000001);
#1806=VECTOR('',#5895,0.210000000000001);
#1807=VECTOR('',#5902,0.210000000000001);
#1808=VECTOR('',#5909,0.21);
#1809=VECTOR('',#5916,0.21);
#1810=VECTOR('',#5923,0.210000000000001);
#1811=VECTOR('',#5930,0.210000000000001);
#1812=VECTOR('',#5937,0.210000000000001);
#1813=VECTOR('',#5944,0.21);
#1814=VECTOR('',#5951,0.21);
#1815=VECTOR('',#5958,0.21);
#1816=VECTOR('',#5965,0.21);
#1817=VECTOR('',#5972,0.210000000000001);
#1818=VECTOR('',#5979,0.210000000000001);
#1819=VECTOR('',#5984,1.);
#1820=VECTOR('',#5985,1.);
#1821=VECTOR('',#5986,1.);
#1822=VECTOR('',#5987,1.);
#1823=VECTOR('',#5990,1.);
#1824=VECTOR('',#5991,1.);
#1825=VECTOR('',#5992,1.);
#1826=VECTOR('',#5995,1.);
#1827=VECTOR('',#5996,1.);
#1828=VECTOR('',#5997,1.);
#1829=VECTOR('',#6000,1.);
#1830=VECTOR('',#6001,1.);
#1831=VECTOR('',#6012,0.55);
#1832=VECTOR('',#6019,0.6);
#1833=VECTOR('',#6026,0.55);
#1834=VECTOR('',#6033,1.);
#1835=VECTOR('',#6038,1.);
#1836=VECTOR('',#6041,1.);
#1837=VECTOR('',#6044,1.);
#1838=VECTOR('',#6047,1.);
#1839=VECTOR('',#6052,1.);
#1840=VECTOR('',#6055,1.);
#1841=VECTOR('',#6056,1.);
#1842=VECTOR('',#6057,1.);
#1843=VECTOR('',#6058,1.);
#1844=VECTOR('',#6059,1.);
#1845=VECTOR('',#6064,1.);
#1846=VECTOR('',#6065,1.);
#1847=VECTOR('',#6066,1.);
#1848=VECTOR('',#6071,1.);
#1849=VECTOR('',#6072,1.);
#1850=VECTOR('',#6073,1.);
#1851=VECTOR('',#6074,1.);
#1852=VECTOR('',#6075,1.);
#1853=VECTOR('',#6082,0.225);
#1854=VECTOR('',#6087,0.165);
#1855=VECTOR('',#6094,0.275);
#1856=VECTOR('',#6099,0.275);
#1857=VECTOR('',#6104,0.6);
#1858=VECTOR('',#6109,1.);
#1859=VECTOR('',#6110,1.);
#1860=VECTOR('',#6111,1.);
#1861=VECTOR('',#6112,1.);
#1862=VECTOR('',#6113,1.);
#1863=VECTOR('',#6114,1.);
#1864=VECTOR('',#6115,1.);
#1865=VECTOR('',#6116,1.);
#1866=VECTOR('',#6117,1.);
#1867=VECTOR('',#6120,1.);
#1868=VECTOR('',#6121,1.);
#1869=VECTOR('',#6124,1.);
#1870=VECTOR('',#6125,1.);
#1871=VECTOR('',#6128,1.);
#1872=VECTOR('',#6131,1.);
#1873=VECTOR('',#6132,1.);
#1874=VECTOR('',#6135,1.);
#1875=VECTOR('',#6136,1.);
#1876=VECTOR('',#6139,1.);
#1877=VECTOR('',#6140,1.);
#1878=VECTOR('',#6143,1.);
#1879=VECTOR('',#6144,1.);
#1880=VECTOR('',#6147,1.);
#1881=VECTOR('',#6148,1.);
#1882=VECTOR('',#6151,1.);
#1883=VECTOR('',#6158,1.);
#1884=VECTOR('',#6159,1.);
#1885=VECTOR('',#6160,1.);
#1886=VECTOR('',#6161,1.);
#1887=VECTOR('',#6164,1.);
#1888=VECTOR('',#6165,1.);
#1889=VECTOR('',#6166,1.);
#1890=VECTOR('',#6169,1.);
#1891=VECTOR('',#6170,1.);
#1892=VECTOR('',#6171,1.);
#1893=VECTOR('',#6174,1.);
#1894=VECTOR('',#6175,1.);
#1895=VECTOR('',#6176,1.);
#1896=VECTOR('',#6179,1.);
#1897=VECTOR('',#6180,1.);
#1898=VECTOR('',#6181,1.);
#1899=VECTOR('',#6184,1.);
#1900=VECTOR('',#6185,1.);
#1901=VECTOR('',#6202,0.4);
#1902=VECTOR('',#6207,0.425);
#1903=VECTOR('',#6212,0.41);
#1904=VECTOR('',#6221,0.26);
#1905=VECTOR('',#6224,0.25);
#1906=VECTOR('',#6231,0.475);
#1907=VECTOR('',#6242,0.475);
#1908=VECTOR('',#6253,0.275);
#1909=VECTOR('',#6258,0.275);
#1910=VECTOR('',#6261,1.);
#1911=VECTOR('',#6262,1.);
#1912=VECTOR('',#6263,1.);
#1913=VECTOR('',#6264,1.);
#1914=VECTOR('',#6267,1.);
#1915=VECTOR('',#6268,1.);
#1916=VECTOR('',#6269,1.);
#1917=VECTOR('',#6272,1.);
#1918=VECTOR('',#6273,1.);
#1919=VECTOR('',#6274,1.);
#1920=VECTOR('',#6277,1.);
#1921=VECTOR('',#6278,1.);
#1922=VECTOR('',#6287,1.);
#1923=VECTOR('',#6288,1.);
#1924=VECTOR('',#6289,1.);
#1925=VECTOR('',#6290,1.);
#1926=VECTOR('',#6293,1.);
#1927=VECTOR('',#6294,1.);
#1928=VECTOR('',#6295,1.);
#1929=VECTOR('',#6298,1.);
#1930=VECTOR('',#6299,1.);
#1931=VECTOR('',#6300,1.);
#1932=VECTOR('',#6303,1.);
#1933=VECTOR('',#6304,1.);
#1934=VECTOR('',#6315,0.34);
#1935=VECTOR('',#6322,0.275);
#1936=VECTOR('',#6329,0.275);
#1937=VECTOR('',#6336,0.275);
#1938=VECTOR('',#6343,0.275);
#1939=VECTOR('',#6348,1.);
#1940=VECTOR('',#6349,1.);
#1941=VECTOR('',#6350,1.);
#1942=VECTOR('',#6351,1.);
#1943=VECTOR('',#6354,1.);
#1944=VECTOR('',#6355,1.);
#1945=VECTOR('',#6356,1.);
#1946=VECTOR('',#6359,1.);
#1947=VECTOR('',#6360,1.);
#1948=VECTOR('',#6361,1.);
#1949=VECTOR('',#6364,1.);
#1950=VECTOR('',#6367,1.);
#1951=VECTOR('',#6370,1.);
#1952=VECTOR('',#6371,1.);
#1953=VECTOR('',#6372,1.);
#1954=VECTOR('',#6373,1.);
#1955=VECTOR('',#6376,1.);
#1956=VECTOR('',#6377,1.);
#1957=VECTOR('',#6378,1.);
#1958=VECTOR('',#6381,1.);
#1959=VECTOR('',#6382,1.);
#1960=VECTOR('',#6383,1.);
#1961=VECTOR('',#6386,1.);
#1962=VECTOR('',#6387,1.);
#1963=VECTOR('',#6396,1.);
#1964=VECTOR('',#6397,1.);
#1965=VECTOR('',#6398,1.);
#1966=VECTOR('',#6399,1.);
#1967=VECTOR('',#6402,1.);
#1968=VECTOR('',#6403,1.);
#1969=VECTOR('',#6404,1.);
#1970=VECTOR('',#6407,1.);
#1971=VECTOR('',#6408,1.);
#1972=VECTOR('',#6409,1.);
#1973=VECTOR('',#6412,1.);
#1974=VECTOR('',#6413,1.);
#1975=VECTOR('',#6414,1.);
#1976=VECTOR('',#6417,1.);
#1977=VECTOR('',#6418,1.);
#1978=VECTOR('',#6419,1.);
#1979=VECTOR('',#6422,1.);
#1980=VECTOR('',#6423,1.);
#1981=VECTOR('',#6440,0.4);
#1982=VECTOR('',#6445,0.425);
#1983=VECTOR('',#6450,0.41);
#1984=VECTOR('',#6459,0.26);
#1985=VECTOR('',#6462,0.25);
#1986=VECTOR('',#6469,0.4);
#1987=VECTOR('',#6476,0.36);
#1988=VECTOR('',#6483,0.734027674973257);
#1989=VECTOR('',#6486,1.);
#1990=VECTOR('',#6487,1.);
#1991=VECTOR('',#6488,1.);
#1992=VECTOR('',#6491,1.);
#1993=VECTOR('',#6492,1.);
#1994=VECTOR('',#6495,1.);
#1995=VECTOR('',#6496,1.);
#1996=VECTOR('',#6499,1.);
#1997=VECTOR('',#6500,1.);
#1998=VECTOR('',#6503,1.);
#1999=VECTOR('',#6504,1.);
#2000=VECTOR('',#6507,1.);
#2001=VECTOR('',#6516,0.734027674973257);
#2002=VECTOR('',#6523,0.734027674973257);
#2003=VECTOR('',#6526,1.);
#2004=VECTOR('',#6527,1.);
#2005=VECTOR('',#6530,1.);
#2006=VECTOR('',#6533,1.);
#2007=VECTOR('',#6538,0.4);
#2008=VECTOR('',#6543,1.);
#2009=VECTOR('',#6546,1.);
#2010=VECTOR('',#6567,1.);
#2011=VECTOR('',#6574,0.21);
#2012=VECTOR('',#6579,1.);
#2013=VECTOR('',#6584,0.605);
#2014=VECTOR('',#6591,1.1);
#2015=VECTOR('',#6602,1.);
#2016=VECTOR('',#6603,1.);
#2017=VECTOR('',#6604,1.);
#2018=VECTOR('',#6605,1.);
#2019=VECTOR('',#6608,1.);
#2020=VECTOR('',#6609,1.);
#2021=VECTOR('',#6610,1.);
#2022=VECTOR('',#6613,1.);
#2023=VECTOR('',#6614,1.);
#2024=VECTOR('',#6615,1.);
#2025=VECTOR('',#6618,1.);
#2026=VECTOR('',#6619,1.);
#2027=VECTOR('',#6620,1.);
#2028=VECTOR('',#6623,1.);
#2029=VECTOR('',#6624,1.);
#2030=VECTOR('',#6625,1.);
#2031=VECTOR('',#6628,1.);
#2032=VECTOR('',#6629,1.);
#2033=VECTOR('',#6640,0.235);
#2034=VECTOR('',#6645,0.25);
#2035=VECTOR('',#6650,0.2125);
#2036=VECTOR('',#6661,0.165);
#2037=VECTOR('',#6668,0.165);
#2038=VECTOR('',#6675,0.165);
#2039=VECTOR('',#6682,0.165);
#2040=VECTOR('',#6689,0.210000000000001);
#2041=VECTOR('',#6698,0.210000000000001);
#2042=VECTOR('',#6707,0.210000000000001);
#2043=VECTOR('',#6716,0.210000000000001);
#2044=VECTOR('',#6725,1.05);
#2045=VECTOR('',#6732,1.05);
#2046=VECTOR('',#6737,1.);
#2047=VECTOR('',#6738,1.);
#2048=VECTOR('',#6739,1.);
#2049=VECTOR('',#6740,1.);
#2050=VECTOR('',#6743,1.);
#2051=VECTOR('',#6744,1.);
#2052=VECTOR('',#6745,1.);
#2053=VECTOR('',#6748,1.);
#2054=VECTOR('',#6749,1.);
#2055=VECTOR('',#6750,1.);
#2056=VECTOR('',#6753,1.);
#2057=VECTOR('',#6754,1.);
#2058=VECTOR('',#6765,0.25);
#2059=VECTOR('',#6772,0.274999999999999);
#2060=VECTOR('',#6779,0.275);
#2061=VECTOR('',#6786,0.275);
#2062=VECTOR('',#6793,0.274999999999999);
#2063=VECTOR('',#6798,1.);
#2064=VECTOR('',#6799,1.);
#2065=VECTOR('',#6800,1.);
#2066=VECTOR('',#6801,1.);
#2067=VECTOR('',#6804,1.);
#2068=VECTOR('',#6805,1.);
#2069=VECTOR('',#6806,1.);
#2070=VECTOR('',#6809,1.);
#2071=VECTOR('',#6810,1.);
#2072=VECTOR('',#6811,1.);
#2073=VECTOR('',#6814,1.);
#2074=VECTOR('',#6815,1.);
#2075=VECTOR('',#6828,1.);
#2076=VECTOR('',#6829,1.);
#2077=VECTOR('',#6830,1.);
#2078=VECTOR('',#6833,1.);
#2079=VECTOR('',#6834,1.);
#2080=VECTOR('',#6835,1.);
#2081=VECTOR('',#6840,1.);
#2082=VECTOR('',#6841,1.);
#2083=VECTOR('',#6844,1.);
#2084=VECTOR('',#6845,1.);
#2085=VECTOR('',#6858,1.05);
#2086=VECTOR('',#6867,1.);
#2087=VECTOR('',#6876,1.05);
#2088=VECTOR('',#6885,1.);
#2089=VECTOR('',#6894,1.05);
#2090=VECTOR('',#6901,0.9);
#2091=VECTOR('',#6908,1.);
#2092=VECTOR('',#6911,1.);
#2093=VECTOR('',#6914,1.);
#2094=VECTOR('',#6915,1.);
#2095=VECTOR('',#6916,1.);
#2096=VECTOR('',#6923,1.);
#2097=VECTOR('',#6926,1.);
#2098=VECTOR('',#6927,1.);
#2099=VECTOR('',#6938,0.895);
#2100=VECTOR('',#6945,0.605);
#2101=VECTOR('',#6956,0.225);
#2102=VECTOR('',#6963,0.225);
#2103=VECTOR('',#6970,0.225);
#2104=VECTOR('',#6977,0.225);
#2105=VECTOR('',#6984,0.7);
#2106=VECTOR('',#6991,0.7);
#2107=VECTOR('',#6996,1.);
#2108=VECTOR('',#6997,1.);
#2109=VECTOR('',#6998,1.);
#2110=VECTOR('',#6999,1.);
#2111=VECTOR('',#7002,1.);
#2112=VECTOR('',#7003,1.);
#2113=VECTOR('',#7004,1.);
#2114=VECTOR('',#7007,1.);
#2115=VECTOR('',#7008,1.);
#2116=VECTOR('',#7009,1.);
#2117=VECTOR('',#7012,1.);
#2118=VECTOR('',#7013,1.);
#2119=VECTOR('',#7028,0.325);
#2120=VECTOR('',#7033,0.35);
#2121=VECTOR('',#7038,0.335);
#2122=VECTOR('',#7047,0.21);
#2123=VECTOR('',#7052,0.2);
#2124=VECTOR('',#7057,0.18);
#2125=VECTOR('',#7062,1.);
#2126=VECTOR('',#7063,1.);
#2127=VECTOR('',#7064,1.);
#2128=VECTOR('',#7065,1.);
#2129=VECTOR('',#7068,1.);
#2130=VECTOR('',#7069,1.);
#2131=VECTOR('',#7070,1.);
#2132=VECTOR('',#7073,1.);
#2133=VECTOR('',#7074,1.);
#2134=VECTOR('',#7075,1.);
#2135=VECTOR('',#7078,1.);
#2136=VECTOR('',#7079,1.);
#2137=VECTOR('',#7080,1.);
#2138=VECTOR('',#7083,1.);
#2139=VECTOR('',#7084,1.);
#2140=VECTOR('',#7085,1.);
#2141=VECTOR('',#7088,1.);
#2142=VECTOR('',#7089,1.);
#2143=VECTOR('',#7104,0.4);
#2144=VECTOR('',#7109,0.425);
#2145=VECTOR('',#7114,0.41);
#2146=VECTOR('',#7123,0.26);
#2147=VECTOR('',#7128,0.25);
#2148=VECTOR('',#7133,0.225);
#2149=VECTOR('',#7138,1.);
#2150=VECTOR('',#7139,1.);
#2151=VECTOR('',#7140,1.);
#2152=VECTOR('',#7141,1.);
#2153=VECTOR('',#7144,1.);
#2154=VECTOR('',#7145,1.);
#2155=VECTOR('',#7146,1.);
#2156=VECTOR('',#7149,1.);
#2157=VECTOR('',#7150,1.);
#2158=VECTOR('',#7151,1.);
#2159=VECTOR('',#7154,1.);
#2160=VECTOR('',#7155,1.);
#2161=VECTOR('',#7156,1.);
#2162=VECTOR('',#7159,1.);
#2163=VECTOR('',#7160,1.);
#2164=VECTOR('',#7161,1.);
#2165=VECTOR('',#7164,1.);
#2166=VECTOR('',#7165,1.);
#2167=VECTOR('',#7250,0.33);
#2168=VECTOR('',#7257,1.5);
#2169=VECTOR('',#7270,0.32);
#2170=VECTOR('',#7277,0.6);
#2171=VECTOR('',#7294,0.475);
#2172=VECTOR('',#7299,0.5);
#2173=VECTOR('',#7304,0.485);
#2174=VECTOR('',#7313,0.31);
#2175=VECTOR('',#7318,0.3);
#2176=VECTOR('',#7323,0.27);
#2177=VECTOR('',#7328,1.);
#2178=VECTOR('',#7329,1.);
#2179=VECTOR('',#7330,1.);
#2180=VECTOR('',#7331,1.);
#2181=VECTOR('',#7334,1.);
#2182=VECTOR('',#7335,1.);
#2183=VECTOR('',#7336,1.);
#2184=VECTOR('',#7339,1.);
#2185=VECTOR('',#7340,1.);
#2186=VECTOR('',#7341,1.);
#2187=VECTOR('',#7344,1.);
#2188=VECTOR('',#7345,1.);
#2189=VECTOR('',#7346,1.);
#2190=VECTOR('',#7349,1.);
#2191=VECTOR('',#7350,1.);
#2192=VECTOR('',#7351,1.);
#2193=VECTOR('',#7354,1.);
#2194=VECTOR('',#7355,1.);
#2195=CIRCLE('',#5293,0.210000000000001);
#2196=CIRCLE('',#5294,0.210000000000001);
#2197=CIRCLE('',#5296,0.210000000000001);
#2198=CIRCLE('',#5297,0.210000000000001);
#2199=CIRCLE('',#5299,0.210000000000001);
#2200=CIRCLE('',#5300,0.210000000000001);
#2201=CIRCLE('',#5302,0.210000000000001);
#2202=CIRCLE('',#5303,0.210000000000001);
#2203=CIRCLE('',#5305,0.210000000000001);
#2204=CIRCLE('',#5306,0.210000000000001);
#2205=CIRCLE('',#5308,0.21);
#2206=CIRCLE('',#5309,0.21);
#2207=CIRCLE('',#5311,0.21);
#2208=CIRCLE('',#5312,0.21);
#2209=CIRCLE('',#5314,0.210000000000001);
#2210=CIRCLE('',#5315,0.210000000000001);
#2211=CIRCLE('',#5317,0.210000000000001);
#2212=CIRCLE('',#5318,0.210000000000001);
#2213=CIRCLE('',#5320,0.210000000000001);
#2214=CIRCLE('',#5321,0.210000000000001);
#2215=CIRCLE('',#5323,0.21);
#2216=CIRCLE('',#5324,0.21);
#2217=CIRCLE('',#5326,0.21);
#2218=CIRCLE('',#5327,0.21);
#2219=CIRCLE('',#5329,0.21);
#2220=CIRCLE('',#5330,0.21);
#2221=CIRCLE('',#5332,0.21);
#2222=CIRCLE('',#5333,0.21);
#2223=CIRCLE('',#5335,0.210000000000001);
#2224=CIRCLE('',#5336,0.210000000000001);
#2225=CIRCLE('',#5338,0.210000000000001);
#2226=CIRCLE('',#5339,0.210000000000001);
#2227=CIRCLE('',#5348,0.6);
#2228=CIRCLE('',#5349,0.5);
#2229=CIRCLE('',#5351,0.6);
#2230=CIRCLE('',#5354,0.5);
#2231=CIRCLE('',#5358,0.525);
#2232=CIRCLE('',#5360,0.525);
#2233=CIRCLE('',#5362,0.525);
#2234=CIRCLE('',#5363,0.525);
#2235=CIRCLE('',#5366,0.275);
#2236=CIRCLE('',#5368,0.165);
#2237=CIRCLE('',#5370,0.275);
#2238=CIRCLE('',#5372,0.225);
#2239=CIRCLE('',#5373,0.225);
#2240=CIRCLE('',#5375,0.165);
#2241=CIRCLE('',#5377,0.275);
#2242=CIRCLE('',#5379,0.275);
#2243=CIRCLE('',#5381,0.6);
#2244=CIRCLE('',#5382,0.6);
#2245=CIRCLE('',#5404,0.24505);
#2246=CIRCLE('',#5406,0.375);
#2247=CIRCLE('',#5408,0.425);
#2248=CIRCLE('',#5410,0.425);
#2249=CIRCLE('',#5412,0.395);
#2250=CIRCLE('',#5414,0.27);
#2251=CIRCLE('',#5416,0.24505);
#2252=CIRCLE('',#5420,0.475);
#2253=CIRCLE('',#5421,0.475);
#2254=CIRCLE('',#5423,0.275);
#2255=CIRCLE('',#5425,0.475);
#2256=CIRCLE('',#5426,0.475);
#2257=CIRCLE('',#5428,0.275);
#2258=CIRCLE('',#5430,0.275);
#2259=CIRCLE('',#5432,0.275);
#2260=CIRCLE('',#5448,0.34);
#2261=CIRCLE('',#5449,0.34);
#2262=CIRCLE('',#5451,0.275);
#2263=CIRCLE('',#5452,0.275);
#2264=CIRCLE('',#5454,0.275);
#2265=CIRCLE('',#5455,0.275);
#2266=CIRCLE('',#5457,0.275);
#2267=CIRCLE('',#5458,0.275);
#2268=CIRCLE('',#5460,0.275);
#2269=CIRCLE('',#5461,0.275);
#2270=CIRCLE('',#5483,0.24505);
#2271=CIRCLE('',#5485,0.375);
#2272=CIRCLE('',#5487,0.425);
#2273=CIRCLE('',#5489,0.425);
#2274=CIRCLE('',#5491,0.395);
#2275=CIRCLE('',#5493,0.27);
#2276=CIRCLE('',#5495,0.24505);
#2277=CIRCLE('',#5499,0.3933);
#2278=CIRCLE('',#5500,0.3933);
#2279=CIRCLE('',#5502,0.32);
#2280=CIRCLE('',#5505,0.6175);
#2281=CIRCLE('',#5516,0.6175);
#2282=CIRCLE('',#5518,0.6175);
#2283=CIRCLE('',#5523,0.338975);
#2284=CIRCLE('',#5524,0.338975);
#2285=CIRCLE('',#5531,0.125);
#2286=CIRCLE('',#5532,0.125);
#2287=CIRCLE('',#5537,0.21);
#2288=CIRCLE('',#5539,0.21);
#2289=CIRCLE('',#5540,0.21);
#2290=CIRCLE('',#5543,0.605);
#2291=CIRCLE('',#5544,0.605);
#2292=CIRCLE('',#5546,1.1);
#2293=CIRCLE('',#5547,1.1);
#2294=CIRCLE('',#5559,0.22);
#2295=CIRCLE('',#5561,0.24505);
#2296=CIRCLE('',#5563,0.24505);
#2297=CIRCLE('',#5565,0.175);
#2298=CIRCLE('',#5570,0.165);
#2299=CIRCLE('',#5571,0.165);
#2300=CIRCLE('',#5573,0.165);
#2301=CIRCLE('',#5574,0.165);
#2302=CIRCLE('',#5576,0.165);
#2303=CIRCLE('',#5577,0.165);
#2304=CIRCLE('',#5579,0.165);
#2305=CIRCLE('',#5580,0.165);
#2306=CIRCLE('',#5582,0.210000000000001);
#2307=CIRCLE('',#5583,0.210000000000001);
#2308=CIRCLE('',#5586,0.210000000000001);
#2309=CIRCLE('',#5587,0.210000000000001);
#2310=CIRCLE('',#5590,0.210000000000001);
#2311=CIRCLE('',#5591,0.210000000000001);
#2312=CIRCLE('',#5594,0.210000000000001);
#2313=CIRCLE('',#5595,0.210000000000001);
#2314=CIRCLE('',#5598,1.05);
#2315=CIRCLE('',#5599,1.05);
#2316=CIRCLE('',#5601,1.05);
#2317=CIRCLE('',#5602,1.05);
#2318=CIRCLE('',#5611,0.25);
#2319=CIRCLE('',#5612,0.25);
#2320=CIRCLE('',#5614,0.274999999999999);
#2321=CIRCLE('',#5615,0.274999999999999);
#2322=CIRCLE('',#5617,0.275);
#2323=CIRCLE('',#5618,0.275);
#2324=CIRCLE('',#5620,0.275);
#2325=CIRCLE('',#5621,0.275);
#2326=CIRCLE('',#5623,0.274999999999999);
#2327=CIRCLE('',#5624,0.274999999999999);
#2328=CIRCLE('',#5634,0.9);
#2329=CIRCLE('',#5637,0.9);
#2330=CIRCLE('',#5641,1.05);
#2331=CIRCLE('',#5642,0.9);
#2332=CIRCLE('',#5644,1.05);
#2333=CIRCLE('',#5646,1.);
#2334=CIRCLE('',#5648,1.);
#2335=CIRCLE('',#5650,1.05);
#2336=CIRCLE('',#5652,1.05);
#2337=CIRCLE('',#5654,1.);
#2338=CIRCLE('',#5656,1.);
#2339=CIRCLE('',#5658,1.05);
#2340=CIRCLE('',#5660,1.05);
#2341=CIRCLE('',#5662,0.9);
#2342=CIRCLE('',#5666,0.895);
#2343=CIRCLE('',#5667,0.605);
#2344=CIRCLE('',#5670,0.895);
#2345=CIRCLE('',#5671,0.605);
#2346=CIRCLE('',#5674,0.895);
#2347=CIRCLE('',#5675,0.605);
#2348=CIRCLE('',#5677,0.895);
#2349=CIRCLE('',#5679,0.605);
#2350=CIRCLE('',#5685,0.225);
#2351=CIRCLE('',#5686,0.225);
#2352=CIRCLE('',#5688,0.225);
#2353=CIRCLE('',#5689,0.225);
#2354=CIRCLE('',#5691,0.225);
#2355=CIRCLE('',#5692,0.225);
#2356=CIRCLE('',#5694,0.225);
#2357=CIRCLE('',#5695,0.225);
#2358=CIRCLE('',#5697,0.7);
#2359=CIRCLE('',#5698,0.7);
#2360=CIRCLE('',#5700,0.7);
#2361=CIRCLE('',#5701,0.7);
#2362=CIRCLE('',#5710,0.3);
#2363=CIRCLE('',#5712,0.35);
#2364=CIRCLE('',#5714,0.35);
#2365=CIRCLE('',#5716,0.32);
#2366=CIRCLE('',#5718,0.22);
#2367=CIRCLE('',#5720,0.1954);
#2368=CIRCLE('',#5722,0.1954);
#2369=CIRCLE('',#5724,0.16);
#2370=CIRCLE('',#5736,0.375);
#2371=CIRCLE('',#5738,0.425);
#2372=CIRCLE('',#5740,0.425);
#2373=CIRCLE('',#5742,0.395);
#2374=CIRCLE('',#5744,0.27);
#2375=CIRCLE('',#5746,0.24505);
#2376=CIRCLE('',#5748,0.24505);
#2377=CIRCLE('',#5750,0.2);
#2378=CIRCLE('',#5799,0.33);
#2379=CIRCLE('',#5800,0.33);
#2380=CIRCLE('',#5802,1.5);
#2381=CIRCLE('',#5803,1.5);
#2382=CIRCLE('',#5808,0.32);
#2383=CIRCLE('',#5809,0.32);
#2384=CIRCLE('',#5811,0.6);
#2385=CIRCLE('',#5812,0.6);
#2386=CIRCLE('',#5817,0.45);
#2387=CIRCLE('',#5819,0.5);
#2388=CIRCLE('',#5821,0.5);
#2389=CIRCLE('',#5823,0.47);
#2390=CIRCLE('',#5825,0.32);
#2391=CIRCLE('',#5827,0.2942);
#2392=CIRCLE('',#5829,0.2942);
#2393=CIRCLE('',#5831,0.24);
#2394=VERTEX_POINT('',#7410);
#2395=VERTEX_POINT('',#7412);
#2396=VERTEX_POINT('',#7416);
#2397=VERTEX_POINT('',#7418);
#2398=VERTEX_POINT('',#7422);
#2399=VERTEX_POINT('',#7424);
#2400=VERTEX_POINT('',#7428);
#2401=VERTEX_POINT('',#7430);
#2402=VERTEX_POINT('',#7434);
#2403=VERTEX_POINT('',#7436);
#2404=VERTEX_POINT('',#7440);
#2405=VERTEX_POINT('',#7442);
#2406=VERTEX_POINT('',#7446);
#2407=VERTEX_POINT('',#7448);
#2408=VERTEX_POINT('',#7452);
#2409=VERTEX_POINT('',#7454);
#2410=VERTEX_POINT('',#7458);
#2411=VERTEX_POINT('',#7460);
#2412=VERTEX_POINT('',#7464);
#2413=VERTEX_POINT('',#7466);
#2414=VERTEX_POINT('',#7470);
#2415=VERTEX_POINT('',#7472);
#2416=VERTEX_POINT('',#7476);
#2417=VERTEX_POINT('',#7478);
#2418=VERTEX_POINT('',#7482);
#2419=VERTEX_POINT('',#7484);
#2420=VERTEX_POINT('',#7488);
#2421=VERTEX_POINT('',#7490);
#2422=VERTEX_POINT('',#7494);
#2423=VERTEX_POINT('',#7496);
#2424=VERTEX_POINT('',#7500);
#2425=VERTEX_POINT('',#7502);
#2426=VERTEX_POINT('',#7506);
#2427=VERTEX_POINT('',#7507);
#2428=VERTEX_POINT('',#7509);
#2429=VERTEX_POINT('',#7511);
#2430=VERTEX_POINT('',#7515);
#2431=VERTEX_POINT('',#7517);
#2432=VERTEX_POINT('',#7521);
#2433=VERTEX_POINT('',#7523);
#2434=VERTEX_POINT('',#7533);
#2435=VERTEX_POINT('',#7535);
#2436=VERTEX_POINT('',#7539);
#2437=VERTEX_POINT('',#7544);
#2438=VERTEX_POINT('',#7550);
#2439=VERTEX_POINT('',#7551);
#2440=VERTEX_POINT('',#7555);
#2441=VERTEX_POINT('',#7557);
#2442=VERTEX_POINT('',#7561);
#2443=VERTEX_POINT('',#7562);
#2444=VERTEX_POINT('',#7564);
#2445=VERTEX_POINT('',#7566);
#2446=VERTEX_POINT('',#7572);
#2447=VERTEX_POINT('',#7574);
#2448=VERTEX_POINT('',#7576);
#2449=VERTEX_POINT('',#7578);
#2450=VERTEX_POINT('',#7581);
#2451=VERTEX_POINT('',#7584);
#2452=VERTEX_POINT('',#7586);
#2453=VERTEX_POINT('',#7589);
#2454=VERTEX_POINT('',#7592);
#2455=VERTEX_POINT('',#7593);
#2456=VERTEX_POINT('',#7595);
#2457=VERTEX_POINT('',#7598);
#2458=VERTEX_POINT('',#7601);
#2459=VERTEX_POINT('',#7604);
#2460=VERTEX_POINT('',#7606);
#2461=VERTEX_POINT('',#7610);
#2462=VERTEX_POINT('',#7614);
#2463=VERTEX_POINT('',#7618);
#2464=VERTEX_POINT('',#7622);
#2465=VERTEX_POINT('',#7624);
#2466=VERTEX_POINT('',#7628);
#2467=VERTEX_POINT('',#7630);
#2468=VERTEX_POINT('',#7633);
#2469=VERTEX_POINT('',#7635);
#2470=VERTEX_POINT('',#7637);
#2471=VERTEX_POINT('',#7639);
#2472=VERTEX_POINT('',#7641);
#2473=VERTEX_POINT('',#7645);
#2474=VERTEX_POINT('',#7649);
#2475=VERTEX_POINT('',#7655);
#2476=VERTEX_POINT('',#7659);
#2477=VERTEX_POINT('',#7663);
#2478=VERTEX_POINT('',#7667);
#2479=VERTEX_POINT('',#7671);
#2480=VERTEX_POINT('',#7679);
#2481=VERTEX_POINT('',#7680);
#2482=VERTEX_POINT('',#7682);
#2483=VERTEX_POINT('',#7684);
#2484=VERTEX_POINT('',#7688);
#2485=VERTEX_POINT('',#7690);
#2486=VERTEX_POINT('',#7694);
#2487=VERTEX_POINT('',#7696);
#2488=VERTEX_POINT('',#7700);
#2489=VERTEX_POINT('',#7702);
#2490=VERTEX_POINT('',#7706);
#2491=VERTEX_POINT('',#7708);
#2492=VERTEX_POINT('',#7717);
#2493=VERTEX_POINT('',#7720);
#2494=VERTEX_POINT('',#7723);
#2495=VERTEX_POINT('',#7727);
#2496=VERTEX_POINT('',#7731);
#2497=VERTEX_POINT('',#7735);
#2498=VERTEX_POINT('',#7738);
#2499=VERTEX_POINT('',#7745);
#2500=VERTEX_POINT('',#7747);
#2501=VERTEX_POINT('',#7751);
#2502=VERTEX_POINT('',#7754);
#2503=VERTEX_POINT('',#7756);
#2504=VERTEX_POINT('',#7760);
#2505=VERTEX_POINT('',#7763);
#2506=VERTEX_POINT('',#7767);
#2507=VERTEX_POINT('',#7771);
#2508=VERTEX_POINT('',#7772);
#2509=VERTEX_POINT('',#7774);
#2510=VERTEX_POINT('',#7776);
#2511=VERTEX_POINT('',#7780);
#2512=VERTEX_POINT('',#7782);
#2513=VERTEX_POINT('',#7786);
#2514=VERTEX_POINT('',#7788);
#2515=VERTEX_POINT('',#7798);
#2516=VERTEX_POINT('',#7799);
#2517=VERTEX_POINT('',#7801);
#2518=VERTEX_POINT('',#7803);
#2519=VERTEX_POINT('',#7807);
#2520=VERTEX_POINT('',#7809);
#2521=VERTEX_POINT('',#7813);
#2522=VERTEX_POINT('',#7815);
#2523=VERTEX_POINT('',#7825);
#2524=VERTEX_POINT('',#7827);
#2525=VERTEX_POINT('',#7831);
#2526=VERTEX_POINT('',#7833);
#2527=VERTEX_POINT('',#7837);
#2528=VERTEX_POINT('',#7839);
#2529=VERTEX_POINT('',#7843);
#2530=VERTEX_POINT('',#7845);
#2531=VERTEX_POINT('',#7849);
#2532=VERTEX_POINT('',#7851);
#2533=VERTEX_POINT('',#7855);
#2534=VERTEX_POINT('',#7856);
#2535=VERTEX_POINT('',#7858);
#2536=VERTEX_POINT('',#7860);
#2537=VERTEX_POINT('',#7864);
#2538=VERTEX_POINT('',#7866);
#2539=VERTEX_POINT('',#7870);
#2540=VERTEX_POINT('',#7872);
#2541=VERTEX_POINT('',#7880);
#2542=VERTEX_POINT('',#7881);
#2543=VERTEX_POINT('',#7883);
#2544=VERTEX_POINT('',#7885);
#2545=VERTEX_POINT('',#7889);
#2546=VERTEX_POINT('',#7891);
#2547=VERTEX_POINT('',#7895);
#2548=VERTEX_POINT('',#7897);
#2549=VERTEX_POINT('',#7907);
#2550=VERTEX_POINT('',#7908);
#2551=VERTEX_POINT('',#7910);
#2552=VERTEX_POINT('',#7912);
#2553=VERTEX_POINT('',#7916);
#2554=VERTEX_POINT('',#7918);
#2555=VERTEX_POINT('',#7922);
#2556=VERTEX_POINT('',#7924);
#2557=VERTEX_POINT('',#7928);
#2558=VERTEX_POINT('',#7930);
#2559=VERTEX_POINT('',#7934);
#2560=VERTEX_POINT('',#7936);
#2561=VERTEX_POINT('',#7945);
#2562=VERTEX_POINT('',#7948);
#2563=VERTEX_POINT('',#7951);
#2564=VERTEX_POINT('',#7955);
#2565=VERTEX_POINT('',#7959);
#2566=VERTEX_POINT('',#7963);
#2567=VERTEX_POINT('',#7966);
#2568=VERTEX_POINT('',#7973);
#2569=VERTEX_POINT('',#7975);
#2570=VERTEX_POINT('',#7979);
#2571=VERTEX_POINT('',#7984);
#2572=VERTEX_POINT('',#7986);
#2573=VERTEX_POINT('',#7988);
#2574=VERTEX_POINT('',#7992);
#2575=VERTEX_POINT('',#7996);
#2576=VERTEX_POINT('',#8000);
#2577=VERTEX_POINT('',#8004);
#2578=VERTEX_POINT('',#8012);
#2579=VERTEX_POINT('',#8014);
#2580=VERTEX_POINT('',#8018);
#2581=VERTEX_POINT('',#8022);
#2582=VERTEX_POINT('',#8026);
#2583=VERTEX_POINT('',#8030);
#2584=VERTEX_POINT('',#8039);
#2585=VERTEX_POINT('',#8040);
#2586=VERTEX_POINT('',#8044);
#2587=VERTEX_POINT('',#8048);
#2588=VERTEX_POINT('',#8051);
#2589=VERTEX_POINT('',#8055);
#2590=VERTEX_POINT('',#8059);
#2591=VERTEX_POINT('',#8067);
#2592=VERTEX_POINT('',#8069);
#2593=VERTEX_POINT('',#8071);
#2594=VERTEX_POINT('',#8075);
#2595=VERTEX_POINT('',#8079);
#2596=VERTEX_POINT('',#8083);
#2597=VERTEX_POINT('',#8087);
#2598=VERTEX_POINT('',#8102);
#2599=VERTEX_POINT('',#8104);
#2600=VERTEX_POINT('',#9345);
#2601=VERTEX_POINT('',#9347);
#2602=VERTEX_POINT('',#9476);
#2603=VERTEX_POINT('',#9477);
#2604=VERTEX_POINT('',#9481);
#2605=VERTEX_POINT('',#9492);
#2606=VERTEX_POINT('',#9494);
#2607=VERTEX_POINT('',#9496);
#2608=VERTEX_POINT('',#9533);
#2609=VERTEX_POINT('',#9548);
#2610=VERTEX_POINT('',#9550);
#2611=VERTEX_POINT('',#9554);
#2612=VERTEX_POINT('',#9556);
#2613=VERTEX_POINT('',#9563);
#2614=VERTEX_POINT('',#9564);
#2615=VERTEX_POINT('',#9566);
#2616=VERTEX_POINT('',#9568);
#2617=VERTEX_POINT('',#9572);
#2618=VERTEX_POINT('',#9574);
#2619=VERTEX_POINT('',#9578);
#2620=VERTEX_POINT('',#9580);
#2621=VERTEX_POINT('',#9584);
#2622=VERTEX_POINT('',#9586);
#2623=VERTEX_POINT('',#9590);
#2624=VERTEX_POINT('',#9592);
#2625=VERTEX_POINT('',#9600);
#2626=VERTEX_POINT('',#9603);
#2627=VERTEX_POINT('',#9607);
#2628=VERTEX_POINT('',#9611);
#2629=VERTEX_POINT('',#9618);
#2630=VERTEX_POINT('',#9620);
#2631=VERTEX_POINT('',#9624);
#2632=VERTEX_POINT('',#9626);
#2633=VERTEX_POINT('',#9630);
#2634=VERTEX_POINT('',#9632);
#2635=VERTEX_POINT('',#9636);
#2636=VERTEX_POINT('',#9638);
#2637=VERTEX_POINT('',#9642);
#2638=VERTEX_POINT('',#9644);
#2639=VERTEX_POINT('',#9649);
#2640=VERTEX_POINT('',#9651);
#2641=VERTEX_POINT('',#9656);
#2642=VERTEX_POINT('',#9658);
#2643=VERTEX_POINT('',#9663);
#2644=VERTEX_POINT('',#9665);
#2645=VERTEX_POINT('',#9670);
#2646=VERTEX_POINT('',#9672);
#2647=VERTEX_POINT('',#9676);
#2648=VERTEX_POINT('',#9678);
#2649=VERTEX_POINT('',#9682);
#2650=VERTEX_POINT('',#9683);
#2651=VERTEX_POINT('',#9685);
#2652=VERTEX_POINT('',#9687);
#2653=VERTEX_POINT('',#9691);
#2654=VERTEX_POINT('',#9693);
#2655=VERTEX_POINT('',#9697);
#2656=VERTEX_POINT('',#9699);
#2657=VERTEX_POINT('',#9709);
#2658=VERTEX_POINT('',#9711);
#2659=VERTEX_POINT('',#9715);
#2660=VERTEX_POINT('',#9717);
#2661=VERTEX_POINT('',#9721);
#2662=VERTEX_POINT('',#9723);
#2663=VERTEX_POINT('',#9727);
#2664=VERTEX_POINT('',#9729);
#2665=VERTEX_POINT('',#9733);
#2666=VERTEX_POINT('',#9735);
#2667=VERTEX_POINT('',#9739);
#2668=VERTEX_POINT('',#9740);
#2669=VERTEX_POINT('',#9742);
#2670=VERTEX_POINT('',#9744);
#2671=VERTEX_POINT('',#9748);
#2672=VERTEX_POINT('',#9750);
#2673=VERTEX_POINT('',#9754);
#2674=VERTEX_POINT('',#9756);
#2675=VERTEX_POINT('',#9767);
#2676=VERTEX_POINT('',#9768);
#2677=VERTEX_POINT('',#9770);
#2678=VERTEX_POINT('',#9772);
#2679=VERTEX_POINT('',#9776);
#2680=VERTEX_POINT('',#9778);
#2681=VERTEX_POINT('',#9782);
#2682=VERTEX_POINT('',#9784);
#2683=VERTEX_POINT('',#9792);
#2684=VERTEX_POINT('',#9794);
#2685=VERTEX_POINT('',#9797);
#2686=VERTEX_POINT('',#9801);
#2687=VERTEX_POINT('',#9804);
#2688=VERTEX_POINT('',#9808);
#2689=VERTEX_POINT('',#9811);
#2690=VERTEX_POINT('',#9815);
#2691=VERTEX_POINT('',#9818);
#2692=VERTEX_POINT('',#9822);
#2693=VERTEX_POINT('',#9825);
#2694=VERTEX_POINT('',#9829);
#2695=VERTEX_POINT('',#9835);
#2696=VERTEX_POINT('',#9836);
#2697=VERTEX_POINT('',#9838);
#2698=VERTEX_POINT('',#9840);
#2699=VERTEX_POINT('',#9844);
#2700=VERTEX_POINT('',#9846);
#2701=VERTEX_POINT('',#9850);
#2702=VERTEX_POINT('',#9852);
#2703=VERTEX_POINT('',#9859);
#2704=VERTEX_POINT('',#9861);
#2705=VERTEX_POINT('',#9864);
#2706=VERTEX_POINT('',#9868);
#2707=VERTEX_POINT('',#9876);
#2708=VERTEX_POINT('',#9878);
#2709=VERTEX_POINT('',#9882);
#2710=VERTEX_POINT('',#9884);
#2711=VERTEX_POINT('',#9888);
#2712=VERTEX_POINT('',#9890);
#2713=VERTEX_POINT('',#9894);
#2714=VERTEX_POINT('',#9896);
#2715=VERTEX_POINT('',#9900);
#2716=VERTEX_POINT('',#9902);
#2717=VERTEX_POINT('',#9906);
#2718=VERTEX_POINT('',#9908);
#2719=VERTEX_POINT('',#9912);
#2720=VERTEX_POINT('',#9913);
#2721=VERTEX_POINT('',#9915);
#2722=VERTEX_POINT('',#9917);
#2723=VERTEX_POINT('',#9921);
#2724=VERTEX_POINT('',#9923);
#2725=VERTEX_POINT('',#9927);
#2726=VERTEX_POINT('',#9929);
#2727=VERTEX_POINT('',#9939);
#2728=VERTEX_POINT('',#9942);
#2729=VERTEX_POINT('',#9946);
#2730=VERTEX_POINT('',#9950);
#2731=VERTEX_POINT('',#9954);
#2732=VERTEX_POINT('',#9957);
#2733=VERTEX_POINT('',#9961);
#2734=VERTEX_POINT('',#9965);
#2735=VERTEX_POINT('',#9970);
#2736=VERTEX_POINT('',#9971);
#2737=VERTEX_POINT('',#9973);
#2738=VERTEX_POINT('',#9975);
#2739=VERTEX_POINT('',#9979);
#2740=VERTEX_POINT('',#9981);
#2741=VERTEX_POINT('',#9985);
#2742=VERTEX_POINT('',#9987);
#2743=VERTEX_POINT('',#9991);
#2744=VERTEX_POINT('',#9993);
#2745=VERTEX_POINT('',#9997);
#2746=VERTEX_POINT('',#9999);
#2747=VERTEX_POINT('',#10009);
#2748=VERTEX_POINT('',#10012);
#2749=VERTEX_POINT('',#10016);
#2750=VERTEX_POINT('',#10020);
#2751=VERTEX_POINT('',#10024);
#2752=VERTEX_POINT('',#10027);
#2753=VERTEX_POINT('',#10031);
#2754=VERTEX_POINT('',#10035);
#2755=VERTEX_POINT('',#10040);
#2756=VERTEX_POINT('',#10041);
#2757=VERTEX_POINT('',#10043);
#2758=VERTEX_POINT('',#10045);
#2759=VERTEX_POINT('',#10049);
#2760=VERTEX_POINT('',#10051);
#2761=VERTEX_POINT('',#10055);
#2762=VERTEX_POINT('',#10057);
#2763=VERTEX_POINT('',#10061);
#2764=VERTEX_POINT('',#10063);
#2765=VERTEX_POINT('',#10067);
#2766=VERTEX_POINT('',#10069);
#2767=VERTEX_POINT('',#10116);
#2768=VERTEX_POINT('',#10118);
#2769=VERTEX_POINT('',#10122);
#2770=VERTEX_POINT('',#10124);
#2771=VERTEX_POINT('',#10131);
#2772=VERTEX_POINT('',#10133);
#2773=VERTEX_POINT('',#10137);
#2774=VERTEX_POINT('',#10139);
#2775=VERTEX_POINT('',#10146);
#2776=VERTEX_POINT('',#10149);
#2777=VERTEX_POINT('',#10153);
#2778=VERTEX_POINT('',#10157);
#2779=VERTEX_POINT('',#10161);
#2780=VERTEX_POINT('',#10164);
#2781=VERTEX_POINT('',#10168);
#2782=VERTEX_POINT('',#10172);
#2783=VERTEX_POINT('',#10177);
#2784=VERTEX_POINT('',#10178);
#2785=VERTEX_POINT('',#10180);
#2786=VERTEX_POINT('',#10182);
#2787=VERTEX_POINT('',#10186);
#2788=VERTEX_POINT('',#10188);
#2789=VERTEX_POINT('',#10192);
#2790=VERTEX_POINT('',#10194);
#2791=VERTEX_POINT('',#10198);
#2792=VERTEX_POINT('',#10200);
#2793=VERTEX_POINT('',#10204);
#2794=VERTEX_POINT('',#10206);
#2795=EDGE_CURVE('',#2394,#2394,#2195,.T.);
#2796=EDGE_CURVE('',#2394,#2395,#1411,.T.);
#2797=EDGE_CURVE('',#2395,#2395,#2196,.T.);
#2798=EDGE_CURVE('',#2396,#2396,#2197,.T.);
#2799=EDGE_CURVE('',#2396,#2397,#1412,.T.);
#2800=EDGE_CURVE('',#2397,#2397,#2198,.T.);
#2801=EDGE_CURVE('',#2398,#2398,#2199,.T.);
#2802=EDGE_CURVE('',#2398,#2399,#1413,.T.);
#2803=EDGE_CURVE('',#2399,#2399,#2200,.T.);
#2804=EDGE_CURVE('',#2400,#2400,#2201,.T.);
#2805=EDGE_CURVE('',#2400,#2401,#1414,.T.);
#2806=EDGE_CURVE('',#2401,#2401,#2202,.T.);
#2807=EDGE_CURVE('',#2402,#2402,#2203,.T.);
#2808=EDGE_CURVE('',#2402,#2403,#1415,.T.);
#2809=EDGE_CURVE('',#2403,#2403,#2204,.T.);
#2810=EDGE_CURVE('',#2404,#2404,#2205,.T.);
#2811=EDGE_CURVE('',#2404,#2405,#1416,.T.);
#2812=EDGE_CURVE('',#2405,#2405,#2206,.T.);
#2813=EDGE_CURVE('',#2406,#2406,#2207,.T.);
#2814=EDGE_CURVE('',#2406,#2407,#1417,.T.);
#2815=EDGE_CURVE('',#2407,#2407,#2208,.T.);
#2816=EDGE_CURVE('',#2408,#2408,#2209,.T.);
#2817=EDGE_CURVE('',#2408,#2409,#1418,.T.);
#2818=EDGE_CURVE('',#2409,#2409,#2210,.T.);
#2819=EDGE_CURVE('',#2410,#2410,#2211,.T.);
#2820=EDGE_CURVE('',#2410,#2411,#1419,.T.);
#2821=EDGE_CURVE('',#2411,#2411,#2212,.T.);
#2822=EDGE_CURVE('',#2412,#2412,#2213,.T.);
#2823=EDGE_CURVE('',#2412,#2413,#1420,.T.);
#2824=EDGE_CURVE('',#2413,#2413,#2214,.T.);
#2825=EDGE_CURVE('',#2414,#2414,#2215,.T.);
#2826=EDGE_CURVE('',#2414,#2415,#1421,.T.);
#2827=EDGE_CURVE('',#2415,#2415,#2216,.T.);
#2828=EDGE_CURVE('',#2416,#2416,#2217,.T.);
#2829=EDGE_CURVE('',#2416,#2417,#1422,.T.);
#2830=EDGE_CURVE('',#2417,#2417,#2218,.T.);
#2831=EDGE_CURVE('',#2418,#2418,#2219,.T.);
#2832=EDGE_CURVE('',#2418,#2419,#1423,.T.);
#2833=EDGE_CURVE('',#2419,#2419,#2220,.T.);
#2834=EDGE_CURVE('',#2420,#2420,#2221,.T.);
#2835=EDGE_CURVE('',#2420,#2421,#1424,.T.);
#2836=EDGE_CURVE('',#2421,#2421,#2222,.T.);
#2837=EDGE_CURVE('',#2422,#2422,#2223,.T.);
#2838=EDGE_CURVE('',#2422,#2423,#1425,.T.);
#2839=EDGE_CURVE('',#2423,#2423,#2224,.T.);
#2840=EDGE_CURVE('',#2424,#2424,#2225,.T.);
#2841=EDGE_CURVE('',#2424,#2425,#1426,.T.);
#2842=EDGE_CURVE('',#2425,#2425,#2226,.T.);
#2843=EDGE_CURVE('',#2426,#2427,#1427,.T.);
#2844=EDGE_CURVE('',#2427,#2428,#1428,.T.);
#2845=EDGE_CURVE('',#2429,#2428,#1429,.T.);
#2846=EDGE_CURVE('',#2426,#2429,#1430,.T.);
#2847=EDGE_CURVE('',#2430,#2426,#1431,.T.);
#2848=EDGE_CURVE('',#2431,#2429,#1432,.T.);
#2849=EDGE_CURVE('',#2430,#2431,#1433,.T.);
#2850=EDGE_CURVE('',#2432,#2430,#1434,.T.);
#2851=EDGE_CURVE('',#2433,#2431,#1435,.T.);
#2852=EDGE_CURVE('',#2432,#2433,#1436,.T.);
#2853=EDGE_CURVE('',#2427,#2432,#1437,.T.);
#2854=EDGE_CURVE('',#2428,#2433,#1438,.T.);
#2855=EDGE_CURVE('',#2434,#2434,#2227,.T.);
#2856=EDGE_CURVE('',#2434,#2435,#1439,.T.);
#2857=EDGE_CURVE('',#2435,#2435,#2228,.T.);
#2858=EDGE_CURVE('',#2436,#2436,#2229,.T.);
#2859=EDGE_CURVE('',#2436,#2434,#1440,.T.);
#2860=EDGE_CURVE('',#2437,#2437,#2230,.T.);
#2861=EDGE_CURVE('',#2437,#2436,#1441,.T.);
#2862=EDGE_CURVE('',#2438,#2439,#1442,.T.);
#2863=EDGE_CURVE('',#2439,#2438,#2231,.T.);
#2864=EDGE_CURVE('',#2440,#2438,#1443,.T.);
#2865=EDGE_CURVE('',#2441,#2440,#2232,.T.);
#2866=EDGE_CURVE('',#2439,#2441,#1444,.T.);
#2867=EDGE_CURVE('',#2442,#2443,#1445,.T.);
#2868=EDGE_CURVE('',#2442,#2444,#2233,.T.);
#2869=EDGE_CURVE('',#2445,#2444,#1446,.T.);
#2870=EDGE_CURVE('',#2443,#2445,#2234,.T.);
#2871=EDGE_CURVE('',#2444,#2442,#1447,.T.);
#2872=EDGE_CURVE('',#2440,#2446,#1448,.T.);
#2873=EDGE_CURVE('',#2447,#2446,#1449,.T.);
#2874=EDGE_CURVE('',#2447,#2448,#1450,.T.);
#2875=EDGE_CURVE('',#2449,#2448,#1451,.T.);
#2876=EDGE_CURVE('',#2449,#2441,#1452,.T.);
#2877=EDGE_CURVE('',#2450,#2450,#2235,.T.);
#2878=EDGE_CURVE('',#2451,#2449,#1453,.T.);
#2879=EDGE_CURVE('',#2451,#2452,#1454,.T.);
#2880=EDGE_CURVE('',#2446,#2452,#1455,.T.);
#2881=EDGE_CURVE('',#2453,#2453,#2236,.T.);
#2882=EDGE_CURVE('',#2454,#2455,#1456,.T.);
#2883=EDGE_CURVE('',#2456,#2455,#1457,.T.);
#2884=EDGE_CURVE('',#2443,#2456,#1458,.T.);
#2885=EDGE_CURVE('',#2457,#2445,#1459,.T.);
#2886=EDGE_CURVE('',#2454,#2457,#1460,.T.);
#2887=EDGE_CURVE('',#2458,#2458,#2237,.T.);
#2888=EDGE_CURVE('',#2459,#2459,#2238,.T.);
#2889=EDGE_CURVE('',#2459,#2460,#1461,.T.);
#2890=EDGE_CURVE('',#2460,#2460,#2239,.T.);
#2891=EDGE_CURVE('',#2453,#2461,#1462,.T.);
#2892=EDGE_CURVE('',#2461,#2461,#2240,.T.);
#2893=EDGE_CURVE('',#2462,#2462,#2241,.T.);
#2894=EDGE_CURVE('',#2462,#2450,#1463,.T.);
#2895=EDGE_CURVE('',#2463,#2463,#2242,.T.);
#2896=EDGE_CURVE('',#2463,#2458,#1464,.T.);
#2897=EDGE_CURVE('',#2464,#2464,#2243,.T.);
#2898=EDGE_CURVE('',#2464,#2465,#1465,.T.);
#2899=EDGE_CURVE('',#2465,#2465,#2244,.T.);
#2900=EDGE_CURVE('',#2448,#2466,#1466,.T.);
#2901=EDGE_CURVE('',#2466,#2467,#1467,.T.);
#2902=EDGE_CURVE('',#2467,#2454,#1468,.T.);
#2903=EDGE_CURVE('',#2457,#2468,#1469,.T.);
#2904=EDGE_CURVE('',#2468,#2469,#1470,.T.);
#2905=EDGE_CURVE('',#2469,#2470,#1471,.T.);
#2906=EDGE_CURVE('',#2470,#2471,#1472,.T.);
#2907=EDGE_CURVE('',#2471,#2472,#1473,.T.);
#2908=EDGE_CURVE('',#2472,#2451,#1474,.T.);
#2909=EDGE_CURVE('',#2473,#2447,#1475,.T.);
#2910=EDGE_CURVE('',#2466,#2473,#1476,.T.);
#2911=EDGE_CURVE('',#2474,#2473,#1477,.T.);
#2912=EDGE_CURVE('',#2467,#2474,#1478,.T.);
#2913=EDGE_CURVE('',#2455,#2474,#1479,.T.);
#2914=EDGE_CURVE('',#2475,#2456,#1480,.T.);
#2915=EDGE_CURVE('',#2468,#2475,#1481,.T.);
#2916=EDGE_CURVE('',#2476,#2475,#1482,.T.);
#2917=EDGE_CURVE('',#2469,#2476,#1483,.T.);
#2918=EDGE_CURVE('',#2477,#2476,#1484,.T.);
#2919=EDGE_CURVE('',#2470,#2477,#1485,.T.);
#2920=EDGE_CURVE('',#2478,#2477,#1486,.T.);
#2921=EDGE_CURVE('',#2471,#2478,#1487,.T.);
#2922=EDGE_CURVE('',#2479,#2478,#1488,.T.);
#2923=EDGE_CURVE('',#2472,#2479,#1489,.T.);
#2924=EDGE_CURVE('',#2452,#2479,#1490,.T.);
#2925=EDGE_CURVE('',#2480,#2481,#1491,.T.);
#2926=EDGE_CURVE('',#2481,#2482,#1492,.T.);
#2927=EDGE_CURVE('',#2482,#2483,#1493,.T.);
#2928=EDGE_CURVE('',#2480,#2483,#1494,.T.);
#2929=EDGE_CURVE('',#2481,#2484,#1495,.T.);
#2930=EDGE_CURVE('',#2484,#2485,#1496,.T.);
#2931=EDGE_CURVE('',#2485,#2482,#1497,.T.);
#2932=EDGE_CURVE('',#2484,#2486,#1498,.T.);
#2933=EDGE_CURVE('',#2486,#2487,#1499,.T.);
#2934=EDGE_CURVE('',#2487,#2485,#1500,.T.);
#2935=EDGE_CURVE('',#2486,#2488,#1501,.T.);
#2936=EDGE_CURVE('',#2488,#2489,#1502,.T.);
#2937=EDGE_CURVE('',#2489,#2487,#1503,.T.);
#2938=EDGE_CURVE('',#2488,#2490,#1504,.T.);
#2939=EDGE_CURVE('',#2490,#2491,#1505,.T.);
#2940=EDGE_CURVE('',#2491,#2489,#1506,.T.);
#2941=EDGE_CURVE('',#2490,#2480,#1507,.T.);
#2942=EDGE_CURVE('',#2483,#2491,#1508,.T.);
#2943=EDGE_CURVE('',#2492,#2492,#2245,.T.);
#2944=EDGE_CURVE('',#2493,#2493,#2246,.T.);
#2945=EDGE_CURVE('',#2494,#2494,#2247,.T.);
#2946=EDGE_CURVE('',#2494,#2493,#1509,.T.);
#2947=EDGE_CURVE('',#2495,#2495,#2248,.T.);
#2948=EDGE_CURVE('',#2495,#2494,#1510,.T.);
#2949=EDGE_CURVE('',#2496,#2496,#2249,.T.);
#2950=EDGE_CURVE('',#2496,#2495,#1511,.T.);
#2951=EDGE_CURVE('',#2497,#2497,#2250,.T.);
#2952=EDGE_CURVE('',#2498,#2498,#2251,.F.);
#2953=EDGE_CURVE('',#2498,#2497,#1512,.T.);
#2954=EDGE_CURVE('',#2492,#2498,#1513,.T.);
#2955=EDGE_CURVE('',#2499,#2499,#2252,.T.);
#2956=EDGE_CURVE('',#2499,#2500,#1514,.T.);
#2957=EDGE_CURVE('',#2500,#2500,#2253,.T.);
#2958=EDGE_CURVE('',#2501,#2501,#2254,.T.);
#2959=EDGE_CURVE('',#2502,#2502,#2255,.T.);
#2960=EDGE_CURVE('',#2502,#2503,#1515,.T.);
#2961=EDGE_CURVE('',#2503,#2503,#2256,.T.);
#2962=EDGE_CURVE('',#2504,#2504,#2257,.T.);
#2963=EDGE_CURVE('',#2505,#2505,#2258,.T.);
#2964=EDGE_CURVE('',#2505,#2501,#1516,.T.);
#2965=EDGE_CURVE('',#2506,#2506,#2259,.T.);
#2966=EDGE_CURVE('',#2506,#2504,#1517,.T.);
#2967=EDGE_CURVE('',#2507,#2508,#1518,.T.);
#2968=EDGE_CURVE('',#2508,#2509,#1519,.T.);
#2969=EDGE_CURVE('',#2510,#2509,#1520,.T.);
#2970=EDGE_CURVE('',#2507,#2510,#1521,.T.);
#2971=EDGE_CURVE('',#2511,#2507,#1522,.T.);
#2972=EDGE_CURVE('',#2512,#2510,#1523,.T.);
#2973=EDGE_CURVE('',#2511,#2512,#1524,.T.);
#2974=EDGE_CURVE('',#2513,#2511,#1525,.T.);
#2975=EDGE_CURVE('',#2514,#2512,#1526,.T.);
#2976=EDGE_CURVE('',#2513,#2514,#1527,.T.);
#2977=EDGE_CURVE('',#2508,#2513,#1528,.T.);
#2978=EDGE_CURVE('',#2509,#2514,#1529,.T.);
#2979=EDGE_CURVE('',#2515,#2516,#1530,.T.);
#2980=EDGE_CURVE('',#2516,#2517,#1531,.T.);
#2981=EDGE_CURVE('',#2518,#2517,#1532,.T.);
#2982=EDGE_CURVE('',#2515,#2518,#1533,.T.);
#2983=EDGE_CURVE('',#2519,#2515,#1534,.T.);
#2984=EDGE_CURVE('',#2520,#2518,#1535,.T.);
#2985=EDGE_CURVE('',#2519,#2520,#1536,.T.);
#2986=EDGE_CURVE('',#2521,#2519,#1537,.T.);
#2987=EDGE_CURVE('',#2522,#2520,#1538,.T.);
#2988=EDGE_CURVE('',#2521,#2522,#1539,.T.);
#2989=EDGE_CURVE('',#2516,#2521,#1540,.T.);
#2990=EDGE_CURVE('',#2517,#2522,#1541,.T.);
#2991=EDGE_CURVE('',#2523,#2523,#2260,.T.);
#2992=EDGE_CURVE('',#2523,#2524,#1542,.T.);
#2993=EDGE_CURVE('',#2524,#2524,#2261,.T.);
#2994=EDGE_CURVE('',#2525,#2525,#2262,.T.);
#2995=EDGE_CURVE('',#2525,#2526,#1543,.T.);
#2996=EDGE_CURVE('',#2526,#2526,#2263,.T.);
#2997=EDGE_CURVE('',#2527,#2527,#2264,.T.);
#2998=EDGE_CURVE('',#2527,#2528,#1544,.T.);
#2999=EDGE_CURVE('',#2528,#2528,#2265,.T.);
#3000=EDGE_CURVE('',#2529,#2529,#2266,.T.);
#3001=EDGE_CURVE('',#2529,#2530,#1545,.T.);
#3002=EDGE_CURVE('',#2530,#2530,#2267,.T.);
#3003=EDGE_CURVE('',#2531,#2531,#2268,.T.);
#3004=EDGE_CURVE('',#2531,#2532,#1546,.T.);
#3005=EDGE_CURVE('',#2532,#2532,#2269,.T.);
#3006=EDGE_CURVE('',#2533,#2534,#1547,.T.);
#3007=EDGE_CURVE('',#2534,#2535,#1548,.T.);
#3008=EDGE_CURVE('',#2536,#2535,#1549,.T.);
#3009=EDGE_CURVE('',#2533,#2536,#1550,.T.);
#3010=EDGE_CURVE('',#2537,#2533,#1551,.T.);
#3011=EDGE_CURVE('',#2538,#2536,#1552,.T.);
#3012=EDGE_CURVE('',#2537,#2538,#1553,.T.);
#3013=EDGE_CURVE('',#2534,#2539,#1554,.T.);
#3014=EDGE_CURVE('',#2540,#2539,#1555,.T.);
#3015=EDGE_CURVE('',#2535,#2540,#1556,.T.);
#3016=EDGE_CURVE('',#2538,#2540,#1557,.T.);
#3017=EDGE_CURVE('',#2539,#2537,#1558,.T.);
#3018=EDGE_CURVE('',#2541,#2542,#1559,.T.);
#3019=EDGE_CURVE('',#2542,#2543,#1560,.T.);
#3020=EDGE_CURVE('',#2544,#2543,#1561,.T.);
#3021=EDGE_CURVE('',#2541,#2544,#1562,.T.);
#3022=EDGE_CURVE('',#2545,#2541,#1563,.T.);
#3023=EDGE_CURVE('',#2546,#2544,#1564,.T.);
#3024=EDGE_CURVE('',#2545,#2546,#1565,.T.);
#3025=EDGE_CURVE('',#2547,#2545,#1566,.T.);
#3026=EDGE_CURVE('',#2548,#2546,#1567,.T.);
#3027=EDGE_CURVE('',#2547,#2548,#1568,.T.);
#3028=EDGE_CURVE('',#2542,#2547,#1569,.T.);
#3029=EDGE_CURVE('',#2543,#2548,#1570,.T.);
#3030=EDGE_CURVE('',#2549,#2550,#1571,.T.);
#3031=EDGE_CURVE('',#2550,#2551,#1572,.T.);
#3032=EDGE_CURVE('',#2551,#2552,#1573,.T.);
#3033=EDGE_CURVE('',#2549,#2552,#1574,.T.);
#3034=EDGE_CURVE('',#2550,#2553,#1575,.T.);
#3035=EDGE_CURVE('',#2553,#2554,#1576,.T.);
#3036=EDGE_CURVE('',#2554,#2551,#1577,.T.);
#3037=EDGE_CURVE('',#2553,#2555,#1578,.T.);
#3038=EDGE_CURVE('',#2555,#2556,#1579,.T.);
#3039=EDGE_CURVE('',#2556,#2554,#1580,.T.);
#3040=EDGE_CURVE('',#2555,#2557,#1581,.T.);
#3041=EDGE_CURVE('',#2557,#2558,#1582,.T.);
#3042=EDGE_CURVE('',#2558,#2556,#1583,.T.);
#3043=EDGE_CURVE('',#2557,#2559,#1584,.T.);
#3044=EDGE_CURVE('',#2559,#2560,#1585,.T.);
#3045=EDGE_CURVE('',#2560,#2558,#1586,.T.);
#3046=EDGE_CURVE('',#2559,#2549,#1587,.T.);
#3047=EDGE_CURVE('',#2552,#2560,#1588,.T.);
#3048=EDGE_CURVE('',#2561,#2561,#2270,.T.);
#3049=EDGE_CURVE('',#2562,#2562,#2271,.T.);
#3050=EDGE_CURVE('',#2563,#2563,#2272,.T.);
#3051=EDGE_CURVE('',#2563,#2562,#1589,.T.);
#3052=EDGE_CURVE('',#2564,#2564,#2273,.T.);
#3053=EDGE_CURVE('',#2564,#2563,#1590,.T.);
#3054=EDGE_CURVE('',#2565,#2565,#2274,.T.);
#3055=EDGE_CURVE('',#2565,#2564,#1591,.T.);
#3056=EDGE_CURVE('',#2566,#2566,#2275,.T.);
#3057=EDGE_CURVE('',#2567,#2567,#2276,.F.);
#3058=EDGE_CURVE('',#2567,#2566,#1592,.T.);
#3059=EDGE_CURVE('',#2561,#2567,#1593,.T.);
#3060=EDGE_CURVE('',#2568,#2568,#2277,.F.);
#3061=EDGE_CURVE('',#2568,#2569,#1594,.T.);
#3062=EDGE_CURVE('',#2569,#2569,#2278,.F.);
#3063=EDGE_CURVE('',#2570,#2570,#2279,.T.);
#3064=EDGE_CURVE('',#2570,#2568,#1595,.T.);
#3065=EDGE_CURVE('',#2571,#2571,#2280,.T.);
#3066=EDGE_CURVE('',#2571,#2572,#1596,.T.);
#3067=EDGE_CURVE('',#2573,#2572,#265,.T.);
#3068=EDGE_CURVE('',#2574,#2573,#266,.T.);
#3069=EDGE_CURVE('',#2575,#2574,#267,.T.);
#3070=EDGE_CURVE('',#2576,#2575,#268,.T.);
#3071=EDGE_CURVE('',#2577,#2576,#269,.T.);
#3072=EDGE_CURVE('',#2572,#2577,#270,.T.);
#3073=EDGE_CURVE('',#2578,#2576,#1597,.T.);
#3074=EDGE_CURVE('',#2578,#2579,#1598,.T.);
#3075=EDGE_CURVE('',#2579,#2577,#1599,.T.);
#3076=EDGE_CURVE('',#2580,#2575,#1600,.T.);
#3077=EDGE_CURVE('',#2580,#2578,#1601,.T.);
#3078=EDGE_CURVE('',#2581,#2574,#1602,.T.);
#3079=EDGE_CURVE('',#2581,#2580,#1603,.T.);
#3080=EDGE_CURVE('',#2582,#2573,#1604,.T.);
#3081=EDGE_CURVE('',#2582,#2581,#1605,.T.);
#3082=EDGE_CURVE('',#2583,#2572,#1606,.T.);
#3083=EDGE_CURVE('',#2583,#2582,#1607,.T.);
#3084=EDGE_CURVE('',#2579,#2583,#1608,.T.);
#3085=EDGE_CURVE('',#2584,#2585,#271,.T.);
#3086=EDGE_CURVE('',#2586,#2584,#272,.T.);
#3087=EDGE_CURVE('',#2586,#2587,#1609,.T.);
#3088=EDGE_CURVE('',#2587,#2587,#2281,.T.);
#3089=EDGE_CURVE('',#2588,#2586,#273,.T.);
#3090=EDGE_CURVE('',#2589,#2588,#274,.T.);
#3091=EDGE_CURVE('',#2590,#2589,#275,.T.);
#3092=EDGE_CURVE('',#2585,#2590,#276,.T.);
#3093=EDGE_CURVE('',#2591,#2591,#2282,.T.);
#3094=EDGE_CURVE('',#2591,#2592,#1610,.T.);
#3095=EDGE_CURVE('',#2593,#2592,#277,.T.);
#3096=EDGE_CURVE('',#2594,#2593,#278,.T.);
#3097=EDGE_CURVE('',#2595,#2594,#279,.T.);
#3098=EDGE_CURVE('',#2596,#2595,#280,.T.);
#3099=EDGE_CURVE('',#2597,#2596,#281,.T.);
#3100=EDGE_CURVE('',#2592,#2597,#282,.T.);
#3101=EDGE_CURVE('',#2588,#2597,#1611,.T.);
#3102=EDGE_CURVE('',#2589,#2596,#1612,.T.);
#3103=EDGE_CURVE('',#2586,#2592,#1613,.T.);
#3104=EDGE_CURVE('',#2584,#2593,#1614,.T.);
#3105=EDGE_CURVE('',#2598,#2598,#2283,.F.);
#3106=EDGE_CURVE('',#2598,#2599,#1615,.T.);
#3107=EDGE_CURVE('',#2599,#2599,#2284,.F.);
#3108=EDGE_CURVE('',#2585,#2594,#1616,.T.);
#3109=EDGE_CURVE('',#2590,#2595,#1617,.T.);
#3110=EDGE_CURVE('',#2600,#2600,#2285,.T.);
#3111=EDGE_CURVE('',#2600,#2601,#259,.T.);
#3112=EDGE_CURVE('',#2601,#2601,#2286,.T.);
#3113=EDGE_CURVE('',#2602,#2603,#1618,.T.);
#3114=EDGE_CURVE('',#2602,#2603,#2287,.T.);
#3115=EDGE_CURVE('',#2604,#2602,#260,.T.);
#3116=EDGE_CURVE('',#2605,#2604,#2288,.T.);
#3117=EDGE_CURVE('',#2605,#2606,#1619,.T.);
#3118=EDGE_CURVE('',#2607,#2606,#261,.T.);
#3119=EDGE_CURVE('',#2606,#2607,#262,.T.);
#3120=EDGE_CURVE('',#2608,#2605,#2289,.T.);
#3121=EDGE_CURVE('',#2603,#2608,#263,.T.);
#3122=EDGE_CURVE('',#2608,#2604,#1620,.T.);
#3123=EDGE_CURVE('',#2609,#2609,#2290,.T.);
#3124=EDGE_CURVE('',#2609,#2610,#1621,.T.);
#3125=EDGE_CURVE('',#2610,#2610,#2291,.T.);
#3126=EDGE_CURVE('',#2611,#2611,#2292,.T.);
#3127=EDGE_CURVE('',#2611,#2612,#1622,.T.);
#3128=EDGE_CURVE('',#2612,#2612,#2293,.T.);
#3129=EDGE_CURVE('',#2613,#2614,#1623,.T.);
#3130=EDGE_CURVE('',#2613,#2615,#1624,.T.);
#3131=EDGE_CURVE('',#2615,#2616,#1625,.T.);
#3132=EDGE_CURVE('',#2614,#2616,#1626,.T.);
#3133=EDGE_CURVE('',#2617,#2613,#1627,.T.);
#3134=EDGE_CURVE('',#2617,#2618,#1628,.T.);
#3135=EDGE_CURVE('',#2618,#2615,#1629,.T.);
#3136=EDGE_CURVE('',#2619,#2617,#1630,.T.);
#3137=EDGE_CURVE('',#2619,#2620,#1631,.T.);
#3138=EDGE_CURVE('',#2620,#2618,#1632,.T.);
#3139=EDGE_CURVE('',#2621,#2619,#1633,.T.);
#3140=EDGE_CURVE('',#2621,#2622,#1634,.T.);
#3141=EDGE_CURVE('',#2622,#2620,#1635,.T.);
#3142=EDGE_CURVE('',#2623,#2621,#1636,.T.);
#3143=EDGE_CURVE('',#2623,#2624,#1637,.T.);
#3144=EDGE_CURVE('',#2624,#2622,#1638,.T.);
#3145=EDGE_CURVE('',#2614,#2623,#1639,.T.);
#3146=EDGE_CURVE('',#2616,#2624,#1640,.T.);
#3147=EDGE_CURVE('',#2625,#2625,#2294,.T.);
#3148=EDGE_CURVE('',#2626,#2626,#2295,.T.);
#3149=EDGE_CURVE('',#2626,#2625,#1641,.T.);
#3150=EDGE_CURVE('',#2627,#2627,#2296,.F.);
#3151=EDGE_CURVE('',#2627,#2626,#1642,.T.);
#3152=EDGE_CURVE('',#2628,#2628,#2297,.T.);
#3153=EDGE_CURVE('',#2628,#2627,#1643,.T.);
#3154=EDGE_CURVE('',#2629,#2629,#2298,.T.);
#3155=EDGE_CURVE('',#2629,#2630,#1644,.T.);
#3156=EDGE_CURVE('',#2630,#2630,#2299,.T.);
#3157=EDGE_CURVE('',#2631,#2631,#2300,.T.);
#3158=EDGE_CURVE('',#2631,#2632,#1645,.T.);
#3159=EDGE_CURVE('',#2632,#2632,#2301,.T.);
#3160=EDGE_CURVE('',#2633,#2633,#2302,.T.);
#3161=EDGE_CURVE('',#2633,#2634,#1646,.T.);
#3162=EDGE_CURVE('',#2634,#2634,#2303,.T.);
#3163=EDGE_CURVE('',#2635,#2635,#2304,.T.);
#3164=EDGE_CURVE('',#2635,#2636,#1647,.T.);
#3165=EDGE_CURVE('',#2636,#2636,#2305,.T.);
#3166=EDGE_CURVE('',#2637,#2637,#2306,.T.);
#3167=EDGE_CURVE('',#2637,#2638,#1648,.T.);
#3168=EDGE_CURVE('',#2638,#2638,#2307,.T.);
#3169=EDGE_CURVE('',#2639,#2639,#2308,.T.);
#3170=EDGE_CURVE('',#2639,#2640,#1649,.T.);
#3171=EDGE_CURVE('',#2640,#2640,#2309,.T.);
#3172=EDGE_CURVE('',#2641,#2641,#2310,.T.);
#3173=EDGE_CURVE('',#2641,#2642,#1650,.T.);
#3174=EDGE_CURVE('',#2642,#2642,#2311,.T.);
#3175=EDGE_CURVE('',#2643,#2643,#2312,.T.);
#3176=EDGE_CURVE('',#2643,#2644,#1651,.T.);
#3177=EDGE_CURVE('',#2644,#2644,#2313,.T.);
#3178=EDGE_CURVE('',#2645,#2645,#2314,.T.);
#3179=EDGE_CURVE('',#2645,#2646,#1652,.T.);
#3180=EDGE_CURVE('',#2646,#2646,#2315,.T.);
#3181=EDGE_CURVE('',#2647,#2647,#2316,.T.);
#3182=EDGE_CURVE('',#2647,#2648,#1653,.T.);
#3183=EDGE_CURVE('',#2648,#2648,#2317,.T.);
#3184=EDGE_CURVE('',#2649,#2650,#1654,.T.);
#3185=EDGE_CURVE('',#2650,#2651,#1655,.T.);
#3186=EDGE_CURVE('',#2652,#2651,#1656,.T.);
#3187=EDGE_CURVE('',#2649,#2652,#1657,.T.);
#3188=EDGE_CURVE('',#2653,#2649,#1658,.T.);
#3189=EDGE_CURVE('',#2654,#2652,#1659,.T.);
#3190=EDGE_CURVE('',#2653,#2654,#1660,.T.);
#3191=EDGE_CURVE('',#2655,#2653,#1661,.T.);
#3192=EDGE_CURVE('',#2656,#2654,#1662,.T.);
#3193=EDGE_CURVE('',#2655,#2656,#1663,.T.);
#3194=EDGE_CURVE('',#2650,#2655,#1664,.T.);
#3195=EDGE_CURVE('',#2651,#2656,#1665,.T.);
#3196=EDGE_CURVE('',#2657,#2657,#2318,.T.);
#3197=EDGE_CURVE('',#2657,#2658,#1666,.T.);
#3198=EDGE_CURVE('',#2658,#2658,#2319,.T.);
#3199=EDGE_CURVE('',#2659,#2659,#2320,.T.);
#3200=EDGE_CURVE('',#2659,#2660,#1667,.T.);
#3201=EDGE_CURVE('',#2660,#2660,#2321,.T.);
#3202=EDGE_CURVE('',#2661,#2661,#2322,.T.);
#3203=EDGE_CURVE('',#2661,#2662,#1668,.T.);
#3204=EDGE_CURVE('',#2662,#2662,#2323,.T.);
#3205=EDGE_CURVE('',#2663,#2663,#2324,.T.);
#3206=EDGE_CURVE('',#2663,#2664,#1669,.T.);
#3207=EDGE_CURVE('',#2664,#2664,#2325,.T.);
#3208=EDGE_CURVE('',#2665,#2665,#2326,.T.);
#3209=EDGE_CURVE('',#2665,#2666,#1670,.T.);
#3210=EDGE_CURVE('',#2666,#2666,#2327,.T.);
#3211=EDGE_CURVE('',#2667,#2668,#1671,.T.);
#3212=EDGE_CURVE('',#2668,#2669,#1672,.T.);
#3213=EDGE_CURVE('',#2670,#2669,#1673,.T.);
#3214=EDGE_CURVE('',#2667,#2670,#1674,.T.);
#3215=EDGE_CURVE('',#2671,#2667,#1675,.T.);
#3216=EDGE_CURVE('',#2672,#2670,#1676,.T.);
#3217=EDGE_CURVE('',#2671,#2672,#1677,.T.);
#3218=EDGE_CURVE('',#2673,#2671,#1678,.T.);
#3219=EDGE_CURVE('',#2674,#2672,#1679,.T.);
#3220=EDGE_CURVE('',#2673,#2674,#1680,.T.);
#3221=EDGE_CURVE('',#2668,#2673,#1681,.T.);
#3222=EDGE_CURVE('',#2669,#2674,#1682,.T.);
#3223=EDGE_CURVE('',#2675,#2676,#2328,.T.);
#3224=EDGE_CURVE('',#2677,#2675,#1683,.T.);
#3225=EDGE_CURVE('',#2678,#2677,#1684,.T.);
#3226=EDGE_CURVE('',#2676,#2678,#1685,.T.);
#3227=EDGE_CURVE('',#2676,#2679,#1686,.T.);
#3228=EDGE_CURVE('',#2680,#2678,#1687,.T.);
#3229=EDGE_CURVE('',#2680,#2679,#1688,.T.);
#3230=EDGE_CURVE('',#2679,#2681,#2329,.T.);
#3231=EDGE_CURVE('',#2682,#2680,#1689,.T.);
#3232=EDGE_CURVE('',#2681,#2682,#1690,.T.);
#3233=EDGE_CURVE('',#2681,#2675,#1691,.T.);
#3234=EDGE_CURVE('',#2682,#2677,#1692,.T.);
#3235=EDGE_CURVE('',#2683,#2683,#2330,.T.);
#3236=EDGE_CURVE('',#2684,#2684,#2331,.T.);
#3237=EDGE_CURVE('',#2685,#2685,#2332,.T.);
#3238=EDGE_CURVE('',#2685,#2683,#1693,.T.);
#3239=EDGE_CURVE('',#2686,#2686,#2333,.T.);
#3240=EDGE_CURVE('',#2687,#2687,#2334,.T.);
#3241=EDGE_CURVE('',#2687,#2686,#1694,.T.);
#3242=EDGE_CURVE('',#2688,#2688,#2335,.T.);
#3243=EDGE_CURVE('',#2689,#2689,#2336,.T.);
#3244=EDGE_CURVE('',#2689,#2688,#1695,.T.);
#3245=EDGE_CURVE('',#2690,#2690,#2337,.T.);
#3246=EDGE_CURVE('',#2691,#2691,#2338,.T.);
#3247=EDGE_CURVE('',#2691,#2690,#1696,.T.);
#3248=EDGE_CURVE('',#2692,#2692,#2339,.T.);
#3249=EDGE_CURVE('',#2693,#2693,#2340,.T.);
#3250=EDGE_CURVE('',#2693,#2692,#1697,.T.);
#3251=EDGE_CURVE('',#2694,#2694,#2341,.T.);
#3252=EDGE_CURVE('',#2694,#2684,#1698,.T.);
#3253=EDGE_CURVE('',#2695,#2696,#2342,.T.);
#3254=EDGE_CURVE('',#2697,#2695,#1699,.T.);
#3255=EDGE_CURVE('',#2698,#2697,#2343,.T.);
#3256=EDGE_CURVE('',#2696,#2698,#1700,.T.);
#3257=EDGE_CURVE('',#2696,#2699,#1701,.T.);
#3258=EDGE_CURVE('',#2700,#2698,#1702,.T.);
#3259=EDGE_CURVE('',#2700,#2699,#1703,.T.);
#3260=EDGE_CURVE('',#2699,#2701,#2344,.T.);
#3261=EDGE_CURVE('',#2702,#2700,#2345,.T.);
#3262=EDGE_CURVE('',#2701,#2702,#1704,.T.);
#3263=EDGE_CURVE('',#2701,#2695,#1705,.T.);
#3264=EDGE_CURVE('',#2697,#2702,#1706,.T.);
#3265=EDGE_CURVE('',#2703,#2703,#2346,.T.);
#3266=EDGE_CURVE('',#2704,#2704,#2347,.T.);
#3267=EDGE_CURVE('',#2705,#2705,#2348,.T.);
#3268=EDGE_CURVE('',#2705,#2703,#1707,.T.);
#3269=EDGE_CURVE('',#2706,#2706,#2349,.T.);
#3270=EDGE_CURVE('',#2706,#2704,#1708,.T.);
#3271=EDGE_CURVE('',#2707,#2707,#2350,.T.);
#3272=EDGE_CURVE('',#2707,#2708,#1709,.T.);
#3273=EDGE_CURVE('',#2708,#2708,#2351,.T.);
#3274=EDGE_CURVE('',#2709,#2709,#2352,.T.);
#3275=EDGE_CURVE('',#2709,#2710,#1710,.T.);
#3276=EDGE_CURVE('',#2710,#2710,#2353,.T.);
#3277=EDGE_CURVE('',#2711,#2711,#2354,.T.);
#3278=EDGE_CURVE('',#2711,#2712,#1711,.T.);
#3279=EDGE_CURVE('',#2712,#2712,#2355,.T.);
#3280=EDGE_CURVE('',#2713,#2713,#2356,.T.);
#3281=EDGE_CURVE('',#2713,#2714,#1712,.T.);
#3282=EDGE_CURVE('',#2714,#2714,#2357,.T.);
#3283=EDGE_CURVE('',#2715,#2715,#2358,.T.);
#3284=EDGE_CURVE('',#2715,#2716,#1713,.T.);
#3285=EDGE_CURVE('',#2716,#2716,#2359,.T.);
#3286=EDGE_CURVE('',#2717,#2717,#2360,.T.);
#3287=EDGE_CURVE('',#2717,#2718,#1714,.T.);
#3288=EDGE_CURVE('',#2718,#2718,#2361,.T.);
#3289=EDGE_CURVE('',#2719,#2720,#1715,.T.);
#3290=EDGE_CURVE('',#2720,#2721,#1716,.T.);
#3291=EDGE_CURVE('',#2722,#2721,#1717,.T.);
#3292=EDGE_CURVE('',#2719,#2722,#1718,.T.);
#3293=EDGE_CURVE('',#2723,#2719,#1719,.T.);
#3294=EDGE_CURVE('',#2724,#2722,#1720,.T.);
#3295=EDGE_CURVE('',#2723,#2724,#1721,.T.);
#3296=EDGE_CURVE('',#2725,#2723,#1722,.T.);
#3297=EDGE_CURVE('',#2726,#2724,#1723,.T.);
#3298=EDGE_CURVE('',#2725,#2726,#1724,.T.);
#3299=EDGE_CURVE('',#2720,#2725,#1725,.T.);
#3300=EDGE_CURVE('',#2721,#2726,#1726,.T.);
#3301=EDGE_CURVE('',#2727,#2727,#2362,.T.);
#3302=EDGE_CURVE('',#2728,#2728,#2363,.T.);
#3303=EDGE_CURVE('',#2728,#2727,#1727,.T.);
#3304=EDGE_CURVE('',#2729,#2729,#2364,.T.);
#3305=EDGE_CURVE('',#2729,#2728,#1728,.T.);
#3306=EDGE_CURVE('',#2730,#2730,#2365,.T.);
#3307=EDGE_CURVE('',#2730,#2729,#1729,.T.);
#3308=EDGE_CURVE('',#2731,#2731,#2366,.T.);
#3309=EDGE_CURVE('',#2732,#2732,#2367,.F.);
#3310=EDGE_CURVE('',#2732,#2731,#1730,.T.);
#3311=EDGE_CURVE('',#2733,#2733,#2368,.F.);
#3312=EDGE_CURVE('',#2733,#2732,#1731,.T.);
#3313=EDGE_CURVE('',#2734,#2734,#2369,.T.);
#3314=EDGE_CURVE('',#2734,#2733,#1732,.T.);
#3315=EDGE_CURVE('',#2735,#2736,#1733,.T.);
#3316=EDGE_CURVE('',#2736,#2737,#1734,.T.);
#3317=EDGE_CURVE('',#2737,#2738,#1735,.T.);
#3318=EDGE_CURVE('',#2735,#2738,#1736,.T.);
#3319=EDGE_CURVE('',#2736,#2739,#1737,.T.);
#3320=EDGE_CURVE('',#2739,#2740,#1738,.T.);
#3321=EDGE_CURVE('',#2740,#2737,#1739,.T.);
#3322=EDGE_CURVE('',#2739,#2741,#1740,.T.);
#3323=EDGE_CURVE('',#2741,#2742,#1741,.T.);
#3324=EDGE_CURVE('',#2742,#2740,#1742,.T.);
#3325=EDGE_CURVE('',#2741,#2743,#1743,.T.);
#3326=EDGE_CURVE('',#2743,#2744,#1744,.T.);
#3327=EDGE_CURVE('',#2744,#2742,#1745,.T.);
#3328=EDGE_CURVE('',#2743,#2745,#1746,.T.);
#3329=EDGE_CURVE('',#2745,#2746,#1747,.T.);
#3330=EDGE_CURVE('',#2746,#2744,#1748,.T.);
#3331=EDGE_CURVE('',#2745,#2735,#1749,.T.);
#3332=EDGE_CURVE('',#2738,#2746,#1750,.T.);
#3333=EDGE_CURVE('',#2747,#2747,#2370,.T.);
#3334=EDGE_CURVE('',#2748,#2748,#2371,.T.);
#3335=EDGE_CURVE('',#2748,#2747,#1751,.T.);
#3336=EDGE_CURVE('',#2749,#2749,#2372,.T.);
#3337=EDGE_CURVE('',#2749,#2748,#1752,.T.);
#3338=EDGE_CURVE('',#2750,#2750,#2373,.T.);
#3339=EDGE_CURVE('',#2750,#2749,#1753,.T.);
#3340=EDGE_CURVE('',#2751,#2751,#2374,.T.);
#3341=EDGE_CURVE('',#2752,#2752,#2375,.F.);
#3342=EDGE_CURVE('',#2752,#2751,#1754,.T.);
#3343=EDGE_CURVE('',#2753,#2753,#2376,.F.);
#3344=EDGE_CURVE('',#2753,#2752,#1755,.T.);
#3345=EDGE_CURVE('',#2754,#2754,#2377,.T.);
#3346=EDGE_CURVE('',#2754,#2753,#1756,.T.);
#3347=EDGE_CURVE('',#2755,#2756,#1757,.T.);
#3348=EDGE_CURVE('',#2756,#2757,#1758,.T.);
#3349=EDGE_CURVE('',#2757,#2758,#1759,.T.);
#3350=EDGE_CURVE('',#2755,#2758,#1760,.T.);
#3351=EDGE_CURVE('',#2756,#2759,#1761,.T.);
#3352=EDGE_CURVE('',#2759,#2760,#1762,.T.);
#3353=EDGE_CURVE('',#2760,#2757,#1763,.T.);
#3354=EDGE_CURVE('',#2759,#2761,#1764,.T.);
#3355=EDGE_CURVE('',#2761,#2762,#1765,.T.);
#3356=EDGE_CURVE('',#2762,#2760,#1766,.T.);
#3357=EDGE_CURVE('',#2761,#2763,#1767,.T.);
#3358=EDGE_CURVE('',#2763,#2764,#1768,.T.);
#3359=EDGE_CURVE('',#2764,#2762,#1769,.T.);
#3360=EDGE_CURVE('',#2763,#2765,#1770,.T.);
#3361=EDGE_CURVE('',#2765,#2766,#1771,.T.);
#3362=EDGE_CURVE('',#2766,#2764,#1772,.T.);
#3363=EDGE_CURVE('',#2765,#2755,#1773,.T.);
#3364=EDGE_CURVE('',#2758,#2766,#1774,.T.);
#3365=EDGE_CURVE('',#2767,#2767,#2378,.T.);
#3366=EDGE_CURVE('',#2767,#2768,#1775,.T.);
#3367=EDGE_CURVE('',#2768,#2768,#2379,.T.);
#3368=EDGE_CURVE('',#2769,#2769,#2380,.T.);
#3369=EDGE_CURVE('',#2769,#2770,#1776,.T.);
#3370=EDGE_CURVE('',#2770,#2770,#2381,.T.);
#3371=EDGE_CURVE('',#2771,#2771,#2382,.T.);
#3372=EDGE_CURVE('',#2771,#2772,#1777,.T.);
#3373=EDGE_CURVE('',#2772,#2772,#2383,.T.);
#3374=EDGE_CURVE('',#2773,#2773,#2384,.T.);
#3375=EDGE_CURVE('',#2773,#2774,#1778,.T.);
#3376=EDGE_CURVE('',#2774,#2774,#2385,.T.);
#3377=EDGE_CURVE('',#2775,#2775,#2386,.T.);
#3378=EDGE_CURVE('',#2776,#2776,#2387,.T.);
#3379=EDGE_CURVE('',#2776,#2775,#1779,.T.);
#3380=EDGE_CURVE('',#2777,#2777,#2388,.T.);
#3381=EDGE_CURVE('',#2777,#2776,#1780,.T.);
#3382=EDGE_CURVE('',#2778,#2778,#2389,.T.);
#3383=EDGE_CURVE('',#2778,#2777,#1781,.T.);
#3384=EDGE_CURVE('',#2779,#2779,#2390,.T.);
#3385=EDGE_CURVE('',#2780,#2780,#2391,.F.);
#3386=EDGE_CURVE('',#2780,#2779,#1782,.T.);
#3387=EDGE_CURVE('',#2781,#2781,#2392,.F.);
#3388=EDGE_CURVE('',#2781,#2780,#1783,.T.);
#3389=EDGE_CURVE('',#2782,#2782,#2393,.T.);
#3390=EDGE_CURVE('',#2782,#2781,#1784,.T.);
#3391=EDGE_CURVE('',#2783,#2784,#1785,.T.);
#3392=EDGE_CURVE('',#2784,#2785,#1786,.T.);
#3393=EDGE_CURVE('',#2785,#2786,#1787,.T.);
#3394=EDGE_CURVE('',#2783,#2786,#1788,.T.);
#3395=EDGE_CURVE('',#2784,#2787,#1789,.T.);
#3396=EDGE_CURVE('',#2787,#2788,#1790,.T.);
#3397=EDGE_CURVE('',#2788,#2785,#1791,.T.);
#3398=EDGE_CURVE('',#2787,#2789,#1792,.T.);
#3399=EDGE_CURVE('',#2789,#2790,#1793,.T.);
#3400=EDGE_CURVE('',#2790,#2788,#1794,.T.);
#3401=EDGE_CURVE('',#2789,#2791,#1795,.T.);
#3402=EDGE_CURVE('',#2791,#2792,#1796,.T.);
#3403=EDGE_CURVE('',#2792,#2790,#1797,.T.);
#3404=EDGE_CURVE('',#2791,#2793,#1798,.T.);
#3405=EDGE_CURVE('',#2793,#2794,#1799,.T.);
#3406=EDGE_CURVE('',#2794,#2792,#1800,.T.);
#3407=EDGE_CURVE('',#2793,#2783,#1801,.T.);
#3408=EDGE_CURVE('',#2786,#2794,#1802,.T.);
#3409=ORIENTED_EDGE('',*,*,#2795,.F.);
#3410=ORIENTED_EDGE('',*,*,#2796,.T.);
#3411=ORIENTED_EDGE('',*,*,#2797,.F.);
#3412=ORIENTED_EDGE('',*,*,#2796,.F.);
#3413=ORIENTED_EDGE('',*,*,#2798,.F.);
#3414=ORIENTED_EDGE('',*,*,#2799,.T.);
#3415=ORIENTED_EDGE('',*,*,#2800,.F.);
#3416=ORIENTED_EDGE('',*,*,#2799,.F.);
#3417=ORIENTED_EDGE('',*,*,#2801,.F.);
#3418=ORIENTED_EDGE('',*,*,#2802,.T.);
#3419=ORIENTED_EDGE('',*,*,#2803,.F.);
#3420=ORIENTED_EDGE('',*,*,#2802,.F.);
#3421=ORIENTED_EDGE('',*,*,#2804,.F.);
#3422=ORIENTED_EDGE('',*,*,#2805,.T.);
#3423=ORIENTED_EDGE('',*,*,#2806,.F.);
#3424=ORIENTED_EDGE('',*,*,#2805,.F.);
#3425=ORIENTED_EDGE('',*,*,#2807,.F.);
#3426=ORIENTED_EDGE('',*,*,#2808,.T.);
#3427=ORIENTED_EDGE('',*,*,#2809,.F.);
#3428=ORIENTED_EDGE('',*,*,#2808,.F.);
#3429=ORIENTED_EDGE('',*,*,#2810,.F.);
#3430=ORIENTED_EDGE('',*,*,#2811,.T.);
#3431=ORIENTED_EDGE('',*,*,#2812,.F.);
#3432=ORIENTED_EDGE('',*,*,#2811,.F.);
#3433=ORIENTED_EDGE('',*,*,#2813,.F.);
#3434=ORIENTED_EDGE('',*,*,#2814,.T.);
#3435=ORIENTED_EDGE('',*,*,#2815,.F.);
#3436=ORIENTED_EDGE('',*,*,#2814,.F.);
#3437=ORIENTED_EDGE('',*,*,#2816,.F.);
#3438=ORIENTED_EDGE('',*,*,#2817,.T.);
#3439=ORIENTED_EDGE('',*,*,#2818,.F.);
#3440=ORIENTED_EDGE('',*,*,#2817,.F.);
#3441=ORIENTED_EDGE('',*,*,#2819,.F.);
#3442=ORIENTED_EDGE('',*,*,#2820,.T.);
#3443=ORIENTED_EDGE('',*,*,#2821,.F.);
#3444=ORIENTED_EDGE('',*,*,#2820,.F.);
#3445=ORIENTED_EDGE('',*,*,#2822,.F.);
#3446=ORIENTED_EDGE('',*,*,#2823,.T.);
#3447=ORIENTED_EDGE('',*,*,#2824,.F.);
#3448=ORIENTED_EDGE('',*,*,#2823,.F.);
#3449=ORIENTED_EDGE('',*,*,#2825,.F.);
#3450=ORIENTED_EDGE('',*,*,#2826,.T.);
#3451=ORIENTED_EDGE('',*,*,#2827,.F.);
#3452=ORIENTED_EDGE('',*,*,#2826,.F.);
#3453=ORIENTED_EDGE('',*,*,#2828,.F.);
#3454=ORIENTED_EDGE('',*,*,#2829,.T.);
#3455=ORIENTED_EDGE('',*,*,#2830,.F.);
#3456=ORIENTED_EDGE('',*,*,#2829,.F.);
#3457=ORIENTED_EDGE('',*,*,#2831,.F.);
#3458=ORIENTED_EDGE('',*,*,#2832,.T.);
#3459=ORIENTED_EDGE('',*,*,#2833,.F.);
#3460=ORIENTED_EDGE('',*,*,#2832,.F.);
#3461=ORIENTED_EDGE('',*,*,#2834,.F.);
#3462=ORIENTED_EDGE('',*,*,#2835,.T.);
#3463=ORIENTED_EDGE('',*,*,#2836,.F.);
#3464=ORIENTED_EDGE('',*,*,#2835,.F.);
#3465=ORIENTED_EDGE('',*,*,#2837,.F.);
#3466=ORIENTED_EDGE('',*,*,#2838,.T.);
#3467=ORIENTED_EDGE('',*,*,#2839,.F.);
#3468=ORIENTED_EDGE('',*,*,#2838,.F.);
#3469=ORIENTED_EDGE('',*,*,#2840,.F.);
#3470=ORIENTED_EDGE('',*,*,#2841,.T.);
#3471=ORIENTED_EDGE('',*,*,#2842,.F.);
#3472=ORIENTED_EDGE('',*,*,#2841,.F.);
#3473=ORIENTED_EDGE('',*,*,#2843,.T.);
#3474=ORIENTED_EDGE('',*,*,#2844,.T.);
#3475=ORIENTED_EDGE('',*,*,#2845,.F.);
#3476=ORIENTED_EDGE('',*,*,#2846,.F.);
#3477=ORIENTED_EDGE('',*,*,#2847,.T.);
#3478=ORIENTED_EDGE('',*,*,#2846,.T.);
#3479=ORIENTED_EDGE('',*,*,#2848,.F.);
#3480=ORIENTED_EDGE('',*,*,#2849,.F.);
#3481=ORIENTED_EDGE('',*,*,#2850,.T.);
#3482=ORIENTED_EDGE('',*,*,#2849,.T.);
#3483=ORIENTED_EDGE('',*,*,#2851,.F.);
#3484=ORIENTED_EDGE('',*,*,#2852,.F.);
#3485=ORIENTED_EDGE('',*,*,#2853,.T.);
#3486=ORIENTED_EDGE('',*,*,#2852,.T.);
#3487=ORIENTED_EDGE('',*,*,#2854,.F.);
#3488=ORIENTED_EDGE('',*,*,#2844,.F.);
#3489=ORIENTED_EDGE('',*,*,#2854,.T.);
#3490=ORIENTED_EDGE('',*,*,#2851,.T.);
#3491=ORIENTED_EDGE('',*,*,#2848,.T.);
#3492=ORIENTED_EDGE('',*,*,#2845,.T.);
#3493=ORIENTED_EDGE('',*,*,#2809,.T.);
#3494=ORIENTED_EDGE('',*,*,#2812,.T.);
#3495=ORIENTED_EDGE('',*,*,#2815,.T.);
#3496=ORIENTED_EDGE('',*,*,#2818,.T.);
#3497=ORIENTED_EDGE('',*,*,#2842,.T.);
#3498=ORIENTED_EDGE('',*,*,#2839,.T.);
#3499=ORIENTED_EDGE('',*,*,#2836,.T.);
#3500=ORIENTED_EDGE('',*,*,#2833,.T.);
#3501=ORIENTED_EDGE('',*,*,#2830,.T.);
#3502=ORIENTED_EDGE('',*,*,#2827,.T.);
#3503=ORIENTED_EDGE('',*,*,#2824,.T.);
#3504=ORIENTED_EDGE('',*,*,#2821,.T.);
#3505=ORIENTED_EDGE('',*,*,#2806,.T.);
#3506=ORIENTED_EDGE('',*,*,#2803,.T.);
#3507=ORIENTED_EDGE('',*,*,#2800,.T.);
#3508=ORIENTED_EDGE('',*,*,#2797,.T.);
#3509=ORIENTED_EDGE('',*,*,#2853,.F.);
#3510=ORIENTED_EDGE('',*,*,#2843,.F.);
#3511=ORIENTED_EDGE('',*,*,#2847,.F.);
#3512=ORIENTED_EDGE('',*,*,#2850,.F.);
#3513=ORIENTED_EDGE('',*,*,#2807,.T.);
#3514=ORIENTED_EDGE('',*,*,#2810,.T.);
#3515=ORIENTED_EDGE('',*,*,#2813,.T.);
#3516=ORIENTED_EDGE('',*,*,#2816,.T.);
#3517=ORIENTED_EDGE('',*,*,#2840,.T.);
#3518=ORIENTED_EDGE('',*,*,#2837,.T.);
#3519=ORIENTED_EDGE('',*,*,#2834,.T.);
#3520=ORIENTED_EDGE('',*,*,#2831,.T.);
#3521=ORIENTED_EDGE('',*,*,#2828,.T.);
#3522=ORIENTED_EDGE('',*,*,#2825,.T.);
#3523=ORIENTED_EDGE('',*,*,#2822,.T.);
#3524=ORIENTED_EDGE('',*,*,#2819,.T.);
#3525=ORIENTED_EDGE('',*,*,#2804,.T.);
#3526=ORIENTED_EDGE('',*,*,#2801,.T.);
#3527=ORIENTED_EDGE('',*,*,#2798,.T.);
#3528=ORIENTED_EDGE('',*,*,#2795,.T.);
#3529=ORIENTED_EDGE('',*,*,#2855,.T.);
#3530=ORIENTED_EDGE('',*,*,#2856,.T.);
#3531=ORIENTED_EDGE('',*,*,#2857,.T.);
#3532=ORIENTED_EDGE('',*,*,#2856,.F.);
#3533=ORIENTED_EDGE('',*,*,#2858,.F.);
#3534=ORIENTED_EDGE('',*,*,#2859,.T.);
#3535=ORIENTED_EDGE('',*,*,#2855,.F.);
#3536=ORIENTED_EDGE('',*,*,#2859,.F.);
#3537=ORIENTED_EDGE('',*,*,#2857,.F.);
#3538=ORIENTED_EDGE('',*,*,#2860,.T.);
#3539=ORIENTED_EDGE('',*,*,#2861,.T.);
#3540=ORIENTED_EDGE('',*,*,#2858,.T.);
#3541=ORIENTED_EDGE('',*,*,#2861,.F.);
#3542=ORIENTED_EDGE('',*,*,#2860,.F.);
#3543=ORIENTED_EDGE('',*,*,#2862,.F.);
#3544=ORIENTED_EDGE('',*,*,#2863,.F.);
#3545=ORIENTED_EDGE('',*,*,#2864,.F.);
#3546=ORIENTED_EDGE('',*,*,#2865,.F.);
#3547=ORIENTED_EDGE('',*,*,#2866,.F.);
#3548=ORIENTED_EDGE('',*,*,#2863,.T.);
#3549=ORIENTED_EDGE('',*,*,#2867,.F.);
#3550=ORIENTED_EDGE('',*,*,#2868,.T.);
#3551=ORIENTED_EDGE('',*,*,#2869,.F.);
#3552=ORIENTED_EDGE('',*,*,#2870,.F.);
#3553=ORIENTED_EDGE('',*,*,#2871,.F.);
#3554=ORIENTED_EDGE('',*,*,#2868,.F.);
#3555=ORIENTED_EDGE('',*,*,#2872,.T.);
#3556=ORIENTED_EDGE('',*,*,#2873,.F.);
#3557=ORIENTED_EDGE('',*,*,#2874,.T.);
#3558=ORIENTED_EDGE('',*,*,#2875,.F.);
#3559=ORIENTED_EDGE('',*,*,#2876,.T.);
#3560=ORIENTED_EDGE('',*,*,#2865,.T.);
#3561=ORIENTED_EDGE('',*,*,#2877,.T.);
#3562=ORIENTED_EDGE('',*,*,#2864,.T.);
#3563=ORIENTED_EDGE('',*,*,#2862,.T.);
#3564=ORIENTED_EDGE('',*,*,#2866,.T.);
#3565=ORIENTED_EDGE('',*,*,#2876,.F.);
#3566=ORIENTED_EDGE('',*,*,#2878,.F.);
#3567=ORIENTED_EDGE('',*,*,#2879,.T.);
#3568=ORIENTED_EDGE('',*,*,#2880,.F.);
#3569=ORIENTED_EDGE('',*,*,#2872,.F.);
#3570=ORIENTED_EDGE('',*,*,#2881,.T.);
#3571=ORIENTED_EDGE('',*,*,#2882,.T.);
#3572=ORIENTED_EDGE('',*,*,#2883,.F.);
#3573=ORIENTED_EDGE('',*,*,#2884,.F.);
#3574=ORIENTED_EDGE('',*,*,#2870,.T.);
#3575=ORIENTED_EDGE('',*,*,#2885,.F.);
#3576=ORIENTED_EDGE('',*,*,#2886,.F.);
#3577=ORIENTED_EDGE('',*,*,#2887,.T.);
#3578=ORIENTED_EDGE('',*,*,#2888,.F.);
#3579=ORIENTED_EDGE('',*,*,#2889,.T.);
#3580=ORIENTED_EDGE('',*,*,#2890,.F.);
#3581=ORIENTED_EDGE('',*,*,#2889,.F.);
#3582=ORIENTED_EDGE('',*,*,#2881,.F.);
#3583=ORIENTED_EDGE('',*,*,#2891,.T.);
#3584=ORIENTED_EDGE('',*,*,#2892,.F.);
#3585=ORIENTED_EDGE('',*,*,#2891,.F.);
#3586=ORIENTED_EDGE('',*,*,#2893,.F.);
#3587=ORIENTED_EDGE('',*,*,#2894,.T.);
#3588=ORIENTED_EDGE('',*,*,#2877,.F.);
#3589=ORIENTED_EDGE('',*,*,#2894,.F.);
#3590=ORIENTED_EDGE('',*,*,#2895,.F.);
#3591=ORIENTED_EDGE('',*,*,#2896,.T.);
#3592=ORIENTED_EDGE('',*,*,#2887,.F.);
#3593=ORIENTED_EDGE('',*,*,#2896,.F.);
#3594=ORIENTED_EDGE('',*,*,#2897,.F.);
#3595=ORIENTED_EDGE('',*,*,#2898,.T.);
#3596=ORIENTED_EDGE('',*,*,#2899,.F.);
#3597=ORIENTED_EDGE('',*,*,#2898,.F.);
#3598=ORIENTED_EDGE('',*,*,#2875,.T.);
#3599=ORIENTED_EDGE('',*,*,#2900,.T.);
#3600=ORIENTED_EDGE('',*,*,#2901,.T.);
#3601=ORIENTED_EDGE('',*,*,#2902,.T.);
#3602=ORIENTED_EDGE('',*,*,#2886,.T.);
#3603=ORIENTED_EDGE('',*,*,#2903,.T.);
#3604=ORIENTED_EDGE('',*,*,#2904,.T.);
#3605=ORIENTED_EDGE('',*,*,#2905,.T.);
#3606=ORIENTED_EDGE('',*,*,#2906,.T.);
#3607=ORIENTED_EDGE('',*,*,#2907,.T.);
#3608=ORIENTED_EDGE('',*,*,#2908,.T.);
#3609=ORIENTED_EDGE('',*,*,#2878,.T.);
#3610=ORIENTED_EDGE('',*,*,#2897,.T.);
#3611=ORIENTED_EDGE('',*,*,#2874,.F.);
#3612=ORIENTED_EDGE('',*,*,#2909,.F.);
#3613=ORIENTED_EDGE('',*,*,#2910,.F.);
#3614=ORIENTED_EDGE('',*,*,#2900,.F.);
#3615=ORIENTED_EDGE('',*,*,#2910,.T.);
#3616=ORIENTED_EDGE('',*,*,#2911,.F.);
#3617=ORIENTED_EDGE('',*,*,#2912,.F.);
#3618=ORIENTED_EDGE('',*,*,#2901,.F.);
#3619=ORIENTED_EDGE('',*,*,#2893,.T.);
#3620=ORIENTED_EDGE('',*,*,#2895,.T.);
#3621=ORIENTED_EDGE('',*,*,#2912,.T.);
#3622=ORIENTED_EDGE('',*,*,#2913,.F.);
#3623=ORIENTED_EDGE('',*,*,#2882,.F.);
#3624=ORIENTED_EDGE('',*,*,#2902,.F.);
#3625=ORIENTED_EDGE('',*,*,#2867,.T.);
#3626=ORIENTED_EDGE('',*,*,#2884,.T.);
#3627=ORIENTED_EDGE('',*,*,#2914,.F.);
#3628=ORIENTED_EDGE('',*,*,#2915,.F.);
#3629=ORIENTED_EDGE('',*,*,#2903,.F.);
#3630=ORIENTED_EDGE('',*,*,#2885,.T.);
#3631=ORIENTED_EDGE('',*,*,#2869,.T.);
#3632=ORIENTED_EDGE('',*,*,#2871,.T.);
#3633=ORIENTED_EDGE('',*,*,#2890,.T.);
#3634=ORIENTED_EDGE('',*,*,#2915,.T.);
#3635=ORIENTED_EDGE('',*,*,#2916,.F.);
#3636=ORIENTED_EDGE('',*,*,#2917,.F.);
#3637=ORIENTED_EDGE('',*,*,#2904,.F.);
#3638=ORIENTED_EDGE('',*,*,#2917,.T.);
#3639=ORIENTED_EDGE('',*,*,#2918,.F.);
#3640=ORIENTED_EDGE('',*,*,#2919,.F.);
#3641=ORIENTED_EDGE('',*,*,#2905,.F.);
#3642=ORIENTED_EDGE('',*,*,#2888,.T.);
#3643=ORIENTED_EDGE('',*,*,#2919,.T.);
#3644=ORIENTED_EDGE('',*,*,#2920,.F.);
#3645=ORIENTED_EDGE('',*,*,#2921,.F.);
#3646=ORIENTED_EDGE('',*,*,#2906,.F.);
#3647=ORIENTED_EDGE('',*,*,#2921,.T.);
#3648=ORIENTED_EDGE('',*,*,#2922,.F.);
#3649=ORIENTED_EDGE('',*,*,#2923,.F.);
#3650=ORIENTED_EDGE('',*,*,#2907,.F.);
#3651=ORIENTED_EDGE('',*,*,#2892,.T.);
#3652=ORIENTED_EDGE('',*,*,#2923,.T.);
#3653=ORIENTED_EDGE('',*,*,#2924,.F.);
#3654=ORIENTED_EDGE('',*,*,#2879,.F.);
#3655=ORIENTED_EDGE('',*,*,#2908,.F.);
#3656=ORIENTED_EDGE('',*,*,#2873,.T.);
#3657=ORIENTED_EDGE('',*,*,#2880,.T.);
#3658=ORIENTED_EDGE('',*,*,#2924,.T.);
#3659=ORIENTED_EDGE('',*,*,#2922,.T.);
#3660=ORIENTED_EDGE('',*,*,#2920,.T.);
#3661=ORIENTED_EDGE('',*,*,#2918,.T.);
#3662=ORIENTED_EDGE('',*,*,#2916,.T.);
#3663=ORIENTED_EDGE('',*,*,#2914,.T.);
#3664=ORIENTED_EDGE('',*,*,#2883,.T.);
#3665=ORIENTED_EDGE('',*,*,#2913,.T.);
#3666=ORIENTED_EDGE('',*,*,#2911,.T.);
#3667=ORIENTED_EDGE('',*,*,#2909,.T.);
#3668=ORIENTED_EDGE('',*,*,#2899,.T.);
#3669=ORIENTED_EDGE('',*,*,#2925,.T.);
#3670=ORIENTED_EDGE('',*,*,#2926,.T.);
#3671=ORIENTED_EDGE('',*,*,#2927,.T.);
#3672=ORIENTED_EDGE('',*,*,#2928,.F.);
#3673=ORIENTED_EDGE('',*,*,#2929,.T.);
#3674=ORIENTED_EDGE('',*,*,#2930,.T.);
#3675=ORIENTED_EDGE('',*,*,#2931,.T.);
#3676=ORIENTED_EDGE('',*,*,#2926,.F.);
#3677=ORIENTED_EDGE('',*,*,#2932,.T.);
#3678=ORIENTED_EDGE('',*,*,#2933,.T.);
#3679=ORIENTED_EDGE('',*,*,#2934,.T.);
#3680=ORIENTED_EDGE('',*,*,#2930,.F.);
#3681=ORIENTED_EDGE('',*,*,#2935,.T.);
#3682=ORIENTED_EDGE('',*,*,#2936,.T.);
#3683=ORIENTED_EDGE('',*,*,#2937,.T.);
#3684=ORIENTED_EDGE('',*,*,#2933,.F.);
#3685=ORIENTED_EDGE('',*,*,#2938,.T.);
#3686=ORIENTED_EDGE('',*,*,#2939,.T.);
#3687=ORIENTED_EDGE('',*,*,#2940,.T.);
#3688=ORIENTED_EDGE('',*,*,#2936,.F.);
#3689=ORIENTED_EDGE('',*,*,#2941,.T.);
#3690=ORIENTED_EDGE('',*,*,#2928,.T.);
#3691=ORIENTED_EDGE('',*,*,#2942,.T.);
#3692=ORIENTED_EDGE('',*,*,#2939,.F.);
#3693=ORIENTED_EDGE('',*,*,#2941,.F.);
#3694=ORIENTED_EDGE('',*,*,#2938,.F.);
#3695=ORIENTED_EDGE('',*,*,#2935,.F.);
#3696=ORIENTED_EDGE('',*,*,#2932,.F.);
#3697=ORIENTED_EDGE('',*,*,#2929,.F.);
#3698=ORIENTED_EDGE('',*,*,#2925,.F.);
#3699=ORIENTED_EDGE('',*,*,#2942,.F.);
#3700=ORIENTED_EDGE('',*,*,#2927,.F.);
#3701=ORIENTED_EDGE('',*,*,#2931,.F.);
#3702=ORIENTED_EDGE('',*,*,#2934,.F.);
#3703=ORIENTED_EDGE('',*,*,#2937,.F.);
#3704=ORIENTED_EDGE('',*,*,#2940,.F.);
#3705=ORIENTED_EDGE('',*,*,#2943,.F.);
#3706=ORIENTED_EDGE('',*,*,#2944,.F.);
#3707=ORIENTED_EDGE('',*,*,#2945,.F.);
#3708=ORIENTED_EDGE('',*,*,#2946,.T.);
#3709=ORIENTED_EDGE('',*,*,#2944,.T.);
#3710=ORIENTED_EDGE('',*,*,#2946,.F.);
#3711=ORIENTED_EDGE('',*,*,#2947,.F.);
#3712=ORIENTED_EDGE('',*,*,#2948,.T.);
#3713=ORIENTED_EDGE('',*,*,#2945,.T.);
#3714=ORIENTED_EDGE('',*,*,#2948,.F.);
#3715=ORIENTED_EDGE('',*,*,#2949,.F.);
#3716=ORIENTED_EDGE('',*,*,#2950,.T.);
#3717=ORIENTED_EDGE('',*,*,#2947,.T.);
#3718=ORIENTED_EDGE('',*,*,#2950,.F.);
#3719=ORIENTED_EDGE('',*,*,#2949,.T.);
#3720=ORIENTED_EDGE('',*,*,#2951,.F.);
#3721=ORIENTED_EDGE('',*,*,#2952,.F.);
#3722=ORIENTED_EDGE('',*,*,#2953,.T.);
#3723=ORIENTED_EDGE('',*,*,#2951,.T.);
#3724=ORIENTED_EDGE('',*,*,#2953,.F.);
#3725=ORIENTED_EDGE('',*,*,#2943,.T.);
#3726=ORIENTED_EDGE('',*,*,#2954,.T.);
#3727=ORIENTED_EDGE('',*,*,#2952,.T.);
#3728=ORIENTED_EDGE('',*,*,#2954,.F.);
#3729=ORIENTED_EDGE('',*,*,#2955,.F.);
#3730=ORIENTED_EDGE('',*,*,#2956,.T.);
#3731=ORIENTED_EDGE('',*,*,#2957,.F.);
#3732=ORIENTED_EDGE('',*,*,#2956,.F.);
#3733=ORIENTED_EDGE('',*,*,#2955,.T.);
#3734=ORIENTED_EDGE('',*,*,#2958,.F.);
#3735=ORIENTED_EDGE('',*,*,#2959,.F.);
#3736=ORIENTED_EDGE('',*,*,#2960,.T.);
#3737=ORIENTED_EDGE('',*,*,#2961,.F.);
#3738=ORIENTED_EDGE('',*,*,#2960,.F.);
#3739=ORIENTED_EDGE('',*,*,#2959,.T.);
#3740=ORIENTED_EDGE('',*,*,#2962,.F.);
#3741=ORIENTED_EDGE('',*,*,#2963,.F.);
#3742=ORIENTED_EDGE('',*,*,#2964,.T.);
#3743=ORIENTED_EDGE('',*,*,#2958,.T.);
#3744=ORIENTED_EDGE('',*,*,#2964,.F.);
#3745=ORIENTED_EDGE('',*,*,#2965,.F.);
#3746=ORIENTED_EDGE('',*,*,#2966,.T.);
#3747=ORIENTED_EDGE('',*,*,#2962,.T.);
#3748=ORIENTED_EDGE('',*,*,#2966,.F.);
#3749=ORIENTED_EDGE('',*,*,#2967,.T.);
#3750=ORIENTED_EDGE('',*,*,#2968,.T.);
#3751=ORIENTED_EDGE('',*,*,#2969,.F.);
#3752=ORIENTED_EDGE('',*,*,#2970,.F.);
#3753=ORIENTED_EDGE('',*,*,#2971,.T.);
#3754=ORIENTED_EDGE('',*,*,#2970,.T.);
#3755=ORIENTED_EDGE('',*,*,#2972,.F.);
#3756=ORIENTED_EDGE('',*,*,#2973,.F.);
#3757=ORIENTED_EDGE('',*,*,#2974,.T.);
#3758=ORIENTED_EDGE('',*,*,#2973,.T.);
#3759=ORIENTED_EDGE('',*,*,#2975,.F.);
#3760=ORIENTED_EDGE('',*,*,#2976,.F.);
#3761=ORIENTED_EDGE('',*,*,#2977,.T.);
#3762=ORIENTED_EDGE('',*,*,#2976,.T.);
#3763=ORIENTED_EDGE('',*,*,#2978,.F.);
#3764=ORIENTED_EDGE('',*,*,#2968,.F.);
#3765=ORIENTED_EDGE('',*,*,#2978,.T.);
#3766=ORIENTED_EDGE('',*,*,#2975,.T.);
#3767=ORIENTED_EDGE('',*,*,#2972,.T.);
#3768=ORIENTED_EDGE('',*,*,#2969,.T.);
#3769=ORIENTED_EDGE('',*,*,#2957,.T.);
#3770=ORIENTED_EDGE('',*,*,#2961,.T.);
#3771=ORIENTED_EDGE('',*,*,#2977,.F.);
#3772=ORIENTED_EDGE('',*,*,#2967,.F.);
#3773=ORIENTED_EDGE('',*,*,#2971,.F.);
#3774=ORIENTED_EDGE('',*,*,#2974,.F.);
#3775=ORIENTED_EDGE('',*,*,#2963,.T.);
#3776=ORIENTED_EDGE('',*,*,#2965,.T.);
#3777=ORIENTED_EDGE('',*,*,#2979,.T.);
#3778=ORIENTED_EDGE('',*,*,#2980,.T.);
#3779=ORIENTED_EDGE('',*,*,#2981,.F.);
#3780=ORIENTED_EDGE('',*,*,#2982,.F.);
#3781=ORIENTED_EDGE('',*,*,#2983,.T.);
#3782=ORIENTED_EDGE('',*,*,#2982,.T.);
#3783=ORIENTED_EDGE('',*,*,#2984,.F.);
#3784=ORIENTED_EDGE('',*,*,#2985,.F.);
#3785=ORIENTED_EDGE('',*,*,#2986,.T.);
#3786=ORIENTED_EDGE('',*,*,#2985,.T.);
#3787=ORIENTED_EDGE('',*,*,#2987,.F.);
#3788=ORIENTED_EDGE('',*,*,#2988,.F.);
#3789=ORIENTED_EDGE('',*,*,#2989,.T.);
#3790=ORIENTED_EDGE('',*,*,#2988,.T.);
#3791=ORIENTED_EDGE('',*,*,#2990,.F.);
#3792=ORIENTED_EDGE('',*,*,#2980,.F.);
#3793=ORIENTED_EDGE('',*,*,#2990,.T.);
#3794=ORIENTED_EDGE('',*,*,#2987,.T.);
#3795=ORIENTED_EDGE('',*,*,#2984,.T.);
#3796=ORIENTED_EDGE('',*,*,#2981,.T.);
#3797=ORIENTED_EDGE('',*,*,#2989,.F.);
#3798=ORIENTED_EDGE('',*,*,#2979,.F.);
#3799=ORIENTED_EDGE('',*,*,#2983,.F.);
#3800=ORIENTED_EDGE('',*,*,#2986,.F.);
#3801=ORIENTED_EDGE('',*,*,#2991,.F.);
#3802=ORIENTED_EDGE('',*,*,#2992,.T.);
#3803=ORIENTED_EDGE('',*,*,#2993,.F.);
#3804=ORIENTED_EDGE('',*,*,#2992,.F.);
#3805=ORIENTED_EDGE('',*,*,#2994,.F.);
#3806=ORIENTED_EDGE('',*,*,#2995,.T.);
#3807=ORIENTED_EDGE('',*,*,#2996,.F.);
#3808=ORIENTED_EDGE('',*,*,#2995,.F.);
#3809=ORIENTED_EDGE('',*,*,#2997,.F.);
#3810=ORIENTED_EDGE('',*,*,#2998,.T.);
#3811=ORIENTED_EDGE('',*,*,#2999,.F.);
#3812=ORIENTED_EDGE('',*,*,#2998,.F.);
#3813=ORIENTED_EDGE('',*,*,#3000,.F.);
#3814=ORIENTED_EDGE('',*,*,#3001,.T.);
#3815=ORIENTED_EDGE('',*,*,#3002,.F.);
#3816=ORIENTED_EDGE('',*,*,#3001,.F.);
#3817=ORIENTED_EDGE('',*,*,#3003,.F.);
#3818=ORIENTED_EDGE('',*,*,#3004,.T.);
#3819=ORIENTED_EDGE('',*,*,#3005,.F.);
#3820=ORIENTED_EDGE('',*,*,#3004,.F.);
#3821=ORIENTED_EDGE('',*,*,#3006,.T.);
#3822=ORIENTED_EDGE('',*,*,#3007,.T.);
#3823=ORIENTED_EDGE('',*,*,#3008,.F.);
#3824=ORIENTED_EDGE('',*,*,#3009,.F.);
#3825=ORIENTED_EDGE('',*,*,#3010,.T.);
#3826=ORIENTED_EDGE('',*,*,#3009,.T.);
#3827=ORIENTED_EDGE('',*,*,#3011,.F.);
#3828=ORIENTED_EDGE('',*,*,#3012,.F.);
#3829=ORIENTED_EDGE('',*,*,#3013,.T.);
#3830=ORIENTED_EDGE('',*,*,#3014,.F.);
#3831=ORIENTED_EDGE('',*,*,#3015,.F.);
#3832=ORIENTED_EDGE('',*,*,#3007,.F.);
#3833=ORIENTED_EDGE('',*,*,#3015,.T.);
#3834=ORIENTED_EDGE('',*,*,#3016,.F.);
#3835=ORIENTED_EDGE('',*,*,#3011,.T.);
#3836=ORIENTED_EDGE('',*,*,#3008,.T.);
#3837=ORIENTED_EDGE('',*,*,#2993,.T.);
#3838=ORIENTED_EDGE('',*,*,#3013,.F.);
#3839=ORIENTED_EDGE('',*,*,#3006,.F.);
#3840=ORIENTED_EDGE('',*,*,#3010,.F.);
#3841=ORIENTED_EDGE('',*,*,#3017,.F.);
#3842=ORIENTED_EDGE('',*,*,#2991,.T.);
#3843=ORIENTED_EDGE('',*,*,#3018,.T.);
#3844=ORIENTED_EDGE('',*,*,#3019,.T.);
#3845=ORIENTED_EDGE('',*,*,#3020,.F.);
#3846=ORIENTED_EDGE('',*,*,#3021,.F.);
#3847=ORIENTED_EDGE('',*,*,#3022,.T.);
#3848=ORIENTED_EDGE('',*,*,#3021,.T.);
#3849=ORIENTED_EDGE('',*,*,#3023,.F.);
#3850=ORIENTED_EDGE('',*,*,#3024,.F.);
#3851=ORIENTED_EDGE('',*,*,#3025,.T.);
#3852=ORIENTED_EDGE('',*,*,#3024,.T.);
#3853=ORIENTED_EDGE('',*,*,#3026,.F.);
#3854=ORIENTED_EDGE('',*,*,#3027,.F.);
#3855=ORIENTED_EDGE('',*,*,#3028,.T.);
#3856=ORIENTED_EDGE('',*,*,#3027,.T.);
#3857=ORIENTED_EDGE('',*,*,#3029,.F.);
#3858=ORIENTED_EDGE('',*,*,#3019,.F.);
#3859=ORIENTED_EDGE('',*,*,#3029,.T.);
#3860=ORIENTED_EDGE('',*,*,#3026,.T.);
#3861=ORIENTED_EDGE('',*,*,#3023,.T.);
#3862=ORIENTED_EDGE('',*,*,#3020,.T.);
#3863=ORIENTED_EDGE('',*,*,#3014,.T.);
#3864=ORIENTED_EDGE('',*,*,#3017,.T.);
#3865=ORIENTED_EDGE('',*,*,#3012,.T.);
#3866=ORIENTED_EDGE('',*,*,#3016,.T.);
#3867=ORIENTED_EDGE('',*,*,#3005,.T.);
#3868=ORIENTED_EDGE('',*,*,#3002,.T.);
#3869=ORIENTED_EDGE('',*,*,#2999,.T.);
#3870=ORIENTED_EDGE('',*,*,#2996,.T.);
#3871=ORIENTED_EDGE('',*,*,#3028,.F.);
#3872=ORIENTED_EDGE('',*,*,#3018,.F.);
#3873=ORIENTED_EDGE('',*,*,#3022,.F.);
#3874=ORIENTED_EDGE('',*,*,#3025,.F.);
#3875=ORIENTED_EDGE('',*,*,#2994,.T.);
#3876=ORIENTED_EDGE('',*,*,#2997,.T.);
#3877=ORIENTED_EDGE('',*,*,#3000,.T.);
#3878=ORIENTED_EDGE('',*,*,#3003,.T.);
#3879=ORIENTED_EDGE('',*,*,#3030,.T.);
#3880=ORIENTED_EDGE('',*,*,#3031,.T.);
#3881=ORIENTED_EDGE('',*,*,#3032,.T.);
#3882=ORIENTED_EDGE('',*,*,#3033,.F.);
#3883=ORIENTED_EDGE('',*,*,#3034,.T.);
#3884=ORIENTED_EDGE('',*,*,#3035,.T.);
#3885=ORIENTED_EDGE('',*,*,#3036,.T.);
#3886=ORIENTED_EDGE('',*,*,#3031,.F.);
#3887=ORIENTED_EDGE('',*,*,#3037,.T.);
#3888=ORIENTED_EDGE('',*,*,#3038,.T.);
#3889=ORIENTED_EDGE('',*,*,#3039,.T.);
#3890=ORIENTED_EDGE('',*,*,#3035,.F.);
#3891=ORIENTED_EDGE('',*,*,#3040,.T.);
#3892=ORIENTED_EDGE('',*,*,#3041,.T.);
#3893=ORIENTED_EDGE('',*,*,#3042,.T.);
#3894=ORIENTED_EDGE('',*,*,#3038,.F.);
#3895=ORIENTED_EDGE('',*,*,#3043,.T.);
#3896=ORIENTED_EDGE('',*,*,#3044,.T.);
#3897=ORIENTED_EDGE('',*,*,#3045,.T.);
#3898=ORIENTED_EDGE('',*,*,#3041,.F.);
#3899=ORIENTED_EDGE('',*,*,#3046,.T.);
#3900=ORIENTED_EDGE('',*,*,#3033,.T.);
#3901=ORIENTED_EDGE('',*,*,#3047,.T.);
#3902=ORIENTED_EDGE('',*,*,#3044,.F.);
#3903=ORIENTED_EDGE('',*,*,#3046,.F.);
#3904=ORIENTED_EDGE('',*,*,#3043,.F.);
#3905=ORIENTED_EDGE('',*,*,#3040,.F.);
#3906=ORIENTED_EDGE('',*,*,#3037,.F.);
#3907=ORIENTED_EDGE('',*,*,#3034,.F.);
#3908=ORIENTED_EDGE('',*,*,#3030,.F.);
#3909=ORIENTED_EDGE('',*,*,#3047,.F.);
#3910=ORIENTED_EDGE('',*,*,#3032,.F.);
#3911=ORIENTED_EDGE('',*,*,#3036,.F.);
#3912=ORIENTED_EDGE('',*,*,#3039,.F.);
#3913=ORIENTED_EDGE('',*,*,#3042,.F.);
#3914=ORIENTED_EDGE('',*,*,#3045,.F.);
#3915=ORIENTED_EDGE('',*,*,#3048,.F.);
#3916=ORIENTED_EDGE('',*,*,#3049,.F.);
#3917=ORIENTED_EDGE('',*,*,#3050,.F.);
#3918=ORIENTED_EDGE('',*,*,#3051,.T.);
#3919=ORIENTED_EDGE('',*,*,#3049,.T.);
#3920=ORIENTED_EDGE('',*,*,#3051,.F.);
#3921=ORIENTED_EDGE('',*,*,#3052,.F.);
#3922=ORIENTED_EDGE('',*,*,#3053,.T.);
#3923=ORIENTED_EDGE('',*,*,#3050,.T.);
#3924=ORIENTED_EDGE('',*,*,#3053,.F.);
#3925=ORIENTED_EDGE('',*,*,#3054,.F.);
#3926=ORIENTED_EDGE('',*,*,#3055,.T.);
#3927=ORIENTED_EDGE('',*,*,#3052,.T.);
#3928=ORIENTED_EDGE('',*,*,#3055,.F.);
#3929=ORIENTED_EDGE('',*,*,#3054,.T.);
#3930=ORIENTED_EDGE('',*,*,#3056,.F.);
#3931=ORIENTED_EDGE('',*,*,#3057,.F.);
#3932=ORIENTED_EDGE('',*,*,#3058,.T.);
#3933=ORIENTED_EDGE('',*,*,#3056,.T.);
#3934=ORIENTED_EDGE('',*,*,#3058,.F.);
#3935=ORIENTED_EDGE('',*,*,#3048,.T.);
#3936=ORIENTED_EDGE('',*,*,#3059,.T.);
#3937=ORIENTED_EDGE('',*,*,#3057,.T.);
#3938=ORIENTED_EDGE('',*,*,#3059,.F.);
#3939=ORIENTED_EDGE('',*,*,#3060,.F.);
#3940=ORIENTED_EDGE('',*,*,#3061,.T.);
#3941=ORIENTED_EDGE('',*,*,#3062,.F.);
#3942=ORIENTED_EDGE('',*,*,#3061,.F.);
#3943=ORIENTED_EDGE('',*,*,#3063,.F.);
#3944=ORIENTED_EDGE('',*,*,#3064,.T.);
#3945=ORIENTED_EDGE('',*,*,#3060,.T.);
#3946=ORIENTED_EDGE('',*,*,#3064,.F.);
#3947=ORIENTED_EDGE('',*,*,#3063,.T.);
#3948=ORIENTED_EDGE('',*,*,#3065,.F.);
#3949=ORIENTED_EDGE('',*,*,#3066,.T.);
#3950=ORIENTED_EDGE('',*,*,#3067,.F.);
#3951=ORIENTED_EDGE('',*,*,#3068,.F.);
#3952=ORIENTED_EDGE('',*,*,#3069,.F.);
#3953=ORIENTED_EDGE('',*,*,#3070,.F.);
#3954=ORIENTED_EDGE('',*,*,#3071,.F.);
#3955=ORIENTED_EDGE('',*,*,#3072,.F.);
#3956=ORIENTED_EDGE('',*,*,#3066,.F.);
#3957=ORIENTED_EDGE('',*,*,#3071,.T.);
#3958=ORIENTED_EDGE('',*,*,#3073,.F.);
#3959=ORIENTED_EDGE('',*,*,#3074,.T.);
#3960=ORIENTED_EDGE('',*,*,#3075,.T.);
#3961=ORIENTED_EDGE('',*,*,#3070,.T.);
#3962=ORIENTED_EDGE('',*,*,#3076,.F.);
#3963=ORIENTED_EDGE('',*,*,#3077,.T.);
#3964=ORIENTED_EDGE('',*,*,#3073,.T.);
#3965=ORIENTED_EDGE('',*,*,#3069,.T.);
#3966=ORIENTED_EDGE('',*,*,#3078,.F.);
#3967=ORIENTED_EDGE('',*,*,#3079,.T.);
#3968=ORIENTED_EDGE('',*,*,#3076,.T.);
#3969=ORIENTED_EDGE('',*,*,#3068,.T.);
#3970=ORIENTED_EDGE('',*,*,#3080,.F.);
#3971=ORIENTED_EDGE('',*,*,#3081,.T.);
#3972=ORIENTED_EDGE('',*,*,#3078,.T.);
#3973=ORIENTED_EDGE('',*,*,#3067,.T.);
#3974=ORIENTED_EDGE('',*,*,#3082,.F.);
#3975=ORIENTED_EDGE('',*,*,#3083,.T.);
#3976=ORIENTED_EDGE('',*,*,#3080,.T.);
#3977=ORIENTED_EDGE('',*,*,#3072,.T.);
#3978=ORIENTED_EDGE('',*,*,#3075,.F.);
#3979=ORIENTED_EDGE('',*,*,#3084,.T.);
#3980=ORIENTED_EDGE('',*,*,#3082,.T.);
#3981=ORIENTED_EDGE('',*,*,#3065,.T.);
#3982=ORIENTED_EDGE('',*,*,#3079,.F.);
#3983=ORIENTED_EDGE('',*,*,#3081,.F.);
#3984=ORIENTED_EDGE('',*,*,#3083,.F.);
#3985=ORIENTED_EDGE('',*,*,#3084,.F.);
#3986=ORIENTED_EDGE('',*,*,#3074,.F.);
#3987=ORIENTED_EDGE('',*,*,#3077,.F.);
#3988=ORIENTED_EDGE('',*,*,#3062,.T.);
#3989=ORIENTED_EDGE('',*,*,#3085,.F.);
#3990=ORIENTED_EDGE('',*,*,#3086,.F.);
#3991=ORIENTED_EDGE('',*,*,#3087,.T.);
#3992=ORIENTED_EDGE('',*,*,#3088,.F.);
#3993=ORIENTED_EDGE('',*,*,#3087,.F.);
#3994=ORIENTED_EDGE('',*,*,#3089,.F.);
#3995=ORIENTED_EDGE('',*,*,#3090,.F.);
#3996=ORIENTED_EDGE('',*,*,#3091,.F.);
#3997=ORIENTED_EDGE('',*,*,#3092,.F.);
#3998=ORIENTED_EDGE('',*,*,#3093,.F.);
#3999=ORIENTED_EDGE('',*,*,#3094,.T.);
#4000=ORIENTED_EDGE('',*,*,#3095,.F.);
#4001=ORIENTED_EDGE('',*,*,#3096,.F.);
#4002=ORIENTED_EDGE('',*,*,#3097,.F.);
#4003=ORIENTED_EDGE('',*,*,#3098,.F.);
#4004=ORIENTED_EDGE('',*,*,#3099,.F.);
#4005=ORIENTED_EDGE('',*,*,#3100,.F.);
#4006=ORIENTED_EDGE('',*,*,#3094,.F.);
#4007=ORIENTED_EDGE('',*,*,#3090,.T.);
#4008=ORIENTED_EDGE('',*,*,#3101,.T.);
#4009=ORIENTED_EDGE('',*,*,#3099,.T.);
#4010=ORIENTED_EDGE('',*,*,#3102,.F.);
#4011=ORIENTED_EDGE('',*,*,#3089,.T.);
#4012=ORIENTED_EDGE('',*,*,#3103,.T.);
#4013=ORIENTED_EDGE('',*,*,#3100,.T.);
#4014=ORIENTED_EDGE('',*,*,#3101,.F.);
#4015=ORIENTED_EDGE('',*,*,#3086,.T.);
#4016=ORIENTED_EDGE('',*,*,#3104,.T.);
#4017=ORIENTED_EDGE('',*,*,#3095,.T.);
#4018=ORIENTED_EDGE('',*,*,#3103,.F.);
#4019=ORIENTED_EDGE('',*,*,#3105,.F.);
#4020=ORIENTED_EDGE('',*,*,#3106,.T.);
#4021=ORIENTED_EDGE('',*,*,#3107,.T.);
#4022=ORIENTED_EDGE('',*,*,#3106,.F.);
#4023=ORIENTED_EDGE('',*,*,#3085,.T.);
#4024=ORIENTED_EDGE('',*,*,#3108,.T.);
#4025=ORIENTED_EDGE('',*,*,#3096,.T.);
#4026=ORIENTED_EDGE('',*,*,#3104,.F.);
#4027=ORIENTED_EDGE('',*,*,#3091,.T.);
#4028=ORIENTED_EDGE('',*,*,#3102,.T.);
#4029=ORIENTED_EDGE('',*,*,#3098,.T.);
#4030=ORIENTED_EDGE('',*,*,#3109,.F.);
#4031=ORIENTED_EDGE('',*,*,#3092,.T.);
#4032=ORIENTED_EDGE('',*,*,#3109,.T.);
#4033=ORIENTED_EDGE('',*,*,#3097,.T.);
#4034=ORIENTED_EDGE('',*,*,#3108,.F.);
#4035=ORIENTED_EDGE('',*,*,#3093,.T.);
#4036=ORIENTED_EDGE('',*,*,#3105,.T.);
#4037=ORIENTED_EDGE('',*,*,#3088,.T.);
#4038=ORIENTED_EDGE('',*,*,#3107,.F.);
#4039=ORIENTED_EDGE('',*,*,#3110,.T.);
#4040=ORIENTED_EDGE('',*,*,#3111,.T.);
#4041=ORIENTED_EDGE('',*,*,#3112,.F.);
#4042=ORIENTED_EDGE('',*,*,#3111,.F.);
#4043=ORIENTED_EDGE('',*,*,#3112,.T.);
#4044=ORIENTED_EDGE('',*,*,#3110,.F.);
#4045=ORIENTED_EDGE('',*,*,#3113,.F.);
#4046=ORIENTED_EDGE('',*,*,#3114,.T.);
#4047=ORIENTED_EDGE('',*,*,#3115,.F.);
#4048=ORIENTED_EDGE('',*,*,#3116,.F.);
#4049=ORIENTED_EDGE('',*,*,#3117,.T.);
#4050=ORIENTED_EDGE('',*,*,#3118,.F.);
#4051=ORIENTED_EDGE('',*,*,#3119,.F.);
#4052=ORIENTED_EDGE('',*,*,#3117,.F.);
#4053=ORIENTED_EDGE('',*,*,#3120,.F.);
#4054=ORIENTED_EDGE('',*,*,#3121,.F.);
#4055=ORIENTED_EDGE('',*,*,#3114,.F.);
#4056=ORIENTED_EDGE('',*,*,#3122,.F.);
#4057=ORIENTED_EDGE('',*,*,#3120,.T.);
#4058=ORIENTED_EDGE('',*,*,#3116,.T.);
#4059=ORIENTED_EDGE('',*,*,#3123,.F.);
#4060=ORIENTED_EDGE('',*,*,#3124,.T.);
#4061=ORIENTED_EDGE('',*,*,#3125,.T.);
#4062=ORIENTED_EDGE('',*,*,#3124,.F.);
#4063=ORIENTED_EDGE('',*,*,#3121,.T.);
#4064=ORIENTED_EDGE('',*,*,#3122,.T.);
#4065=ORIENTED_EDGE('',*,*,#3115,.T.);
#4066=ORIENTED_EDGE('',*,*,#3113,.T.);
#4067=ORIENTED_EDGE('',*,*,#3126,.F.);
#4068=ORIENTED_EDGE('',*,*,#3127,.T.);
#4069=ORIENTED_EDGE('',*,*,#3128,.T.);
#4070=ORIENTED_EDGE('',*,*,#3127,.F.);
#4071=ORIENTED_EDGE('',*,*,#3118,.T.);
#4072=ORIENTED_EDGE('',*,*,#3119,.T.);
#4073=ORIENTED_EDGE('',*,*,#3126,.T.);
#4074=ORIENTED_EDGE('',*,*,#3123,.T.);
#4075=ORIENTED_EDGE('',*,*,#3128,.F.);
#4076=ORIENTED_EDGE('',*,*,#3125,.F.);
#4077=ORIENTED_EDGE('',*,*,#3129,.F.);
#4078=ORIENTED_EDGE('',*,*,#3130,.T.);
#4079=ORIENTED_EDGE('',*,*,#3131,.T.);
#4080=ORIENTED_EDGE('',*,*,#3132,.F.);
#4081=ORIENTED_EDGE('',*,*,#3133,.F.);
#4082=ORIENTED_EDGE('',*,*,#3134,.T.);
#4083=ORIENTED_EDGE('',*,*,#3135,.T.);
#4084=ORIENTED_EDGE('',*,*,#3130,.F.);
#4085=ORIENTED_EDGE('',*,*,#3136,.F.);
#4086=ORIENTED_EDGE('',*,*,#3137,.T.);
#4087=ORIENTED_EDGE('',*,*,#3138,.T.);
#4088=ORIENTED_EDGE('',*,*,#3134,.F.);
#4089=ORIENTED_EDGE('',*,*,#3139,.F.);
#4090=ORIENTED_EDGE('',*,*,#3140,.T.);
#4091=ORIENTED_EDGE('',*,*,#3141,.T.);
#4092=ORIENTED_EDGE('',*,*,#3137,.F.);
#4093=ORIENTED_EDGE('',*,*,#3142,.F.);
#4094=ORIENTED_EDGE('',*,*,#3143,.T.);
#4095=ORIENTED_EDGE('',*,*,#3144,.T.);
#4096=ORIENTED_EDGE('',*,*,#3140,.F.);
#4097=ORIENTED_EDGE('',*,*,#3145,.F.);
#4098=ORIENTED_EDGE('',*,*,#3132,.T.);
#4099=ORIENTED_EDGE('',*,*,#3146,.T.);
#4100=ORIENTED_EDGE('',*,*,#3143,.F.);
#4101=ORIENTED_EDGE('',*,*,#3146,.F.);
#4102=ORIENTED_EDGE('',*,*,#3131,.F.);
#4103=ORIENTED_EDGE('',*,*,#3135,.F.);
#4104=ORIENTED_EDGE('',*,*,#3138,.F.);
#4105=ORIENTED_EDGE('',*,*,#3141,.F.);
#4106=ORIENTED_EDGE('',*,*,#3144,.F.);
#4107=ORIENTED_EDGE('',*,*,#3147,.F.);
#4108=ORIENTED_EDGE('',*,*,#3129,.T.);
#4109=ORIENTED_EDGE('',*,*,#3145,.T.);
#4110=ORIENTED_EDGE('',*,*,#3142,.T.);
#4111=ORIENTED_EDGE('',*,*,#3139,.T.);
#4112=ORIENTED_EDGE('',*,*,#3136,.T.);
#4113=ORIENTED_EDGE('',*,*,#3133,.T.);
#4114=ORIENTED_EDGE('',*,*,#3148,.F.);
#4115=ORIENTED_EDGE('',*,*,#3149,.T.);
#4116=ORIENTED_EDGE('',*,*,#3147,.T.);
#4117=ORIENTED_EDGE('',*,*,#3149,.F.);
#4118=ORIENTED_EDGE('',*,*,#3150,.F.);
#4119=ORIENTED_EDGE('',*,*,#3151,.T.);
#4120=ORIENTED_EDGE('',*,*,#3148,.T.);
#4121=ORIENTED_EDGE('',*,*,#3151,.F.);
#4122=ORIENTED_EDGE('',*,*,#3152,.F.);
#4123=ORIENTED_EDGE('',*,*,#3153,.T.);
#4124=ORIENTED_EDGE('',*,*,#3150,.T.);
#4125=ORIENTED_EDGE('',*,*,#3153,.F.);
#4126=ORIENTED_EDGE('',*,*,#3152,.T.);
#4127=ORIENTED_EDGE('',*,*,#3154,.F.);
#4128=ORIENTED_EDGE('',*,*,#3155,.T.);
#4129=ORIENTED_EDGE('',*,*,#3156,.F.);
#4130=ORIENTED_EDGE('',*,*,#3155,.F.);
#4131=ORIENTED_EDGE('',*,*,#3157,.F.);
#4132=ORIENTED_EDGE('',*,*,#3158,.T.);
#4133=ORIENTED_EDGE('',*,*,#3159,.F.);
#4134=ORIENTED_EDGE('',*,*,#3158,.F.);
#4135=ORIENTED_EDGE('',*,*,#3160,.F.);
#4136=ORIENTED_EDGE('',*,*,#3161,.T.);
#4137=ORIENTED_EDGE('',*,*,#3162,.F.);
#4138=ORIENTED_EDGE('',*,*,#3161,.F.);
#4139=ORIENTED_EDGE('',*,*,#3163,.F.);
#4140=ORIENTED_EDGE('',*,*,#3164,.T.);
#4141=ORIENTED_EDGE('',*,*,#3165,.F.);
#4142=ORIENTED_EDGE('',*,*,#3164,.F.);
#4143=ORIENTED_EDGE('',*,*,#3166,.F.);
#4144=ORIENTED_EDGE('',*,*,#3167,.T.);
#4145=ORIENTED_EDGE('',*,*,#3168,.F.);
#4146=ORIENTED_EDGE('',*,*,#3167,.F.);
#4147=ORIENTED_EDGE('',*,*,#3166,.T.);
#4148=ORIENTED_EDGE('',*,*,#3169,.F.);
#4149=ORIENTED_EDGE('',*,*,#3170,.T.);
#4150=ORIENTED_EDGE('',*,*,#3171,.F.);
#4151=ORIENTED_EDGE('',*,*,#3170,.F.);
#4152=ORIENTED_EDGE('',*,*,#3169,.T.);
#4153=ORIENTED_EDGE('',*,*,#3172,.F.);
#4154=ORIENTED_EDGE('',*,*,#3173,.T.);
#4155=ORIENTED_EDGE('',*,*,#3174,.F.);
#4156=ORIENTED_EDGE('',*,*,#3173,.F.);
#4157=ORIENTED_EDGE('',*,*,#3172,.T.);
#4158=ORIENTED_EDGE('',*,*,#3175,.F.);
#4159=ORIENTED_EDGE('',*,*,#3176,.T.);
#4160=ORIENTED_EDGE('',*,*,#3177,.F.);
#4161=ORIENTED_EDGE('',*,*,#3176,.F.);
#4162=ORIENTED_EDGE('',*,*,#3175,.T.);
#4163=ORIENTED_EDGE('',*,*,#3178,.F.);
#4164=ORIENTED_EDGE('',*,*,#3179,.T.);
#4165=ORIENTED_EDGE('',*,*,#3180,.F.);
#4166=ORIENTED_EDGE('',*,*,#3179,.F.);
#4167=ORIENTED_EDGE('',*,*,#3181,.F.);
#4168=ORIENTED_EDGE('',*,*,#3182,.T.);
#4169=ORIENTED_EDGE('',*,*,#3183,.F.);
#4170=ORIENTED_EDGE('',*,*,#3182,.F.);
#4171=ORIENTED_EDGE('',*,*,#3184,.T.);
#4172=ORIENTED_EDGE('',*,*,#3185,.T.);
#4173=ORIENTED_EDGE('',*,*,#3186,.F.);
#4174=ORIENTED_EDGE('',*,*,#3187,.F.);
#4175=ORIENTED_EDGE('',*,*,#3188,.T.);
#4176=ORIENTED_EDGE('',*,*,#3187,.T.);
#4177=ORIENTED_EDGE('',*,*,#3189,.F.);
#4178=ORIENTED_EDGE('',*,*,#3190,.F.);
#4179=ORIENTED_EDGE('',*,*,#3183,.T.);
#4180=ORIENTED_EDGE('',*,*,#3180,.T.);
#4181=ORIENTED_EDGE('',*,*,#3165,.T.);
#4182=ORIENTED_EDGE('',*,*,#3162,.T.);
#4183=ORIENTED_EDGE('',*,*,#3159,.T.);
#4184=ORIENTED_EDGE('',*,*,#3156,.T.);
#4185=ORIENTED_EDGE('',*,*,#3191,.T.);
#4186=ORIENTED_EDGE('',*,*,#3190,.T.);
#4187=ORIENTED_EDGE('',*,*,#3192,.F.);
#4188=ORIENTED_EDGE('',*,*,#3193,.F.);
#4189=ORIENTED_EDGE('',*,*,#3194,.T.);
#4190=ORIENTED_EDGE('',*,*,#3193,.T.);
#4191=ORIENTED_EDGE('',*,*,#3195,.F.);
#4192=ORIENTED_EDGE('',*,*,#3185,.F.);
#4193=ORIENTED_EDGE('',*,*,#3181,.T.);
#4194=ORIENTED_EDGE('',*,*,#3178,.T.);
#4195=ORIENTED_EDGE('',*,*,#3163,.T.);
#4196=ORIENTED_EDGE('',*,*,#3160,.T.);
#4197=ORIENTED_EDGE('',*,*,#3157,.T.);
#4198=ORIENTED_EDGE('',*,*,#3154,.T.);
#4199=ORIENTED_EDGE('',*,*,#3195,.T.);
#4200=ORIENTED_EDGE('',*,*,#3192,.T.);
#4201=ORIENTED_EDGE('',*,*,#3189,.T.);
#4202=ORIENTED_EDGE('',*,*,#3186,.T.);
#4203=ORIENTED_EDGE('',*,*,#3168,.T.);
#4204=ORIENTED_EDGE('',*,*,#3171,.T.);
#4205=ORIENTED_EDGE('',*,*,#3174,.T.);
#4206=ORIENTED_EDGE('',*,*,#3177,.T.);
#4207=ORIENTED_EDGE('',*,*,#3194,.F.);
#4208=ORIENTED_EDGE('',*,*,#3184,.F.);
#4209=ORIENTED_EDGE('',*,*,#3188,.F.);
#4210=ORIENTED_EDGE('',*,*,#3191,.F.);
#4211=ORIENTED_EDGE('',*,*,#3196,.F.);
#4212=ORIENTED_EDGE('',*,*,#3197,.T.);
#4213=ORIENTED_EDGE('',*,*,#3198,.F.);
#4214=ORIENTED_EDGE('',*,*,#3197,.F.);
#4215=ORIENTED_EDGE('',*,*,#3199,.F.);
#4216=ORIENTED_EDGE('',*,*,#3200,.T.);
#4217=ORIENTED_EDGE('',*,*,#3201,.F.);
#4218=ORIENTED_EDGE('',*,*,#3200,.F.);
#4219=ORIENTED_EDGE('',*,*,#3202,.F.);
#4220=ORIENTED_EDGE('',*,*,#3203,.T.);
#4221=ORIENTED_EDGE('',*,*,#3204,.F.);
#4222=ORIENTED_EDGE('',*,*,#3203,.F.);
#4223=ORIENTED_EDGE('',*,*,#3205,.F.);
#4224=ORIENTED_EDGE('',*,*,#3206,.T.);
#4225=ORIENTED_EDGE('',*,*,#3207,.F.);
#4226=ORIENTED_EDGE('',*,*,#3206,.F.);
#4227=ORIENTED_EDGE('',*,*,#3208,.F.);
#4228=ORIENTED_EDGE('',*,*,#3209,.T.);
#4229=ORIENTED_EDGE('',*,*,#3210,.F.);
#4230=ORIENTED_EDGE('',*,*,#3209,.F.);
#4231=ORIENTED_EDGE('',*,*,#3211,.T.);
#4232=ORIENTED_EDGE('',*,*,#3212,.T.);
#4233=ORIENTED_EDGE('',*,*,#3213,.F.);
#4234=ORIENTED_EDGE('',*,*,#3214,.F.);
#4235=ORIENTED_EDGE('',*,*,#3215,.T.);
#4236=ORIENTED_EDGE('',*,*,#3214,.T.);
#4237=ORIENTED_EDGE('',*,*,#3216,.F.);
#4238=ORIENTED_EDGE('',*,*,#3217,.F.);
#4239=ORIENTED_EDGE('',*,*,#3218,.T.);
#4240=ORIENTED_EDGE('',*,*,#3217,.T.);
#4241=ORIENTED_EDGE('',*,*,#3219,.F.);
#4242=ORIENTED_EDGE('',*,*,#3220,.F.);
#4243=ORIENTED_EDGE('',*,*,#3221,.T.);
#4244=ORIENTED_EDGE('',*,*,#3220,.T.);
#4245=ORIENTED_EDGE('',*,*,#3222,.F.);
#4246=ORIENTED_EDGE('',*,*,#3212,.F.);
#4247=ORIENTED_EDGE('',*,*,#3222,.T.);
#4248=ORIENTED_EDGE('',*,*,#3219,.T.);
#4249=ORIENTED_EDGE('',*,*,#3216,.T.);
#4250=ORIENTED_EDGE('',*,*,#3213,.T.);
#4251=ORIENTED_EDGE('',*,*,#3198,.T.);
#4252=ORIENTED_EDGE('',*,*,#3201,.T.);
#4253=ORIENTED_EDGE('',*,*,#3204,.T.);
#4254=ORIENTED_EDGE('',*,*,#3207,.T.);
#4255=ORIENTED_EDGE('',*,*,#3210,.T.);
#4256=ORIENTED_EDGE('',*,*,#3221,.F.);
#4257=ORIENTED_EDGE('',*,*,#3211,.F.);
#4258=ORIENTED_EDGE('',*,*,#3215,.F.);
#4259=ORIENTED_EDGE('',*,*,#3218,.F.);
#4260=ORIENTED_EDGE('',*,*,#3196,.T.);
#4261=ORIENTED_EDGE('',*,*,#3199,.T.);
#4262=ORIENTED_EDGE('',*,*,#3202,.T.);
#4263=ORIENTED_EDGE('',*,*,#3205,.T.);
#4264=ORIENTED_EDGE('',*,*,#3208,.T.);
#4265=ORIENTED_EDGE('',*,*,#3223,.F.);
#4266=ORIENTED_EDGE('',*,*,#3224,.F.);
#4267=ORIENTED_EDGE('',*,*,#3225,.F.);
#4268=ORIENTED_EDGE('',*,*,#3226,.F.);
#4269=ORIENTED_EDGE('',*,*,#3227,.F.);
#4270=ORIENTED_EDGE('',*,*,#3226,.T.);
#4271=ORIENTED_EDGE('',*,*,#3228,.F.);
#4272=ORIENTED_EDGE('',*,*,#3229,.T.);
#4273=ORIENTED_EDGE('',*,*,#3230,.F.);
#4274=ORIENTED_EDGE('',*,*,#3229,.F.);
#4275=ORIENTED_EDGE('',*,*,#3231,.F.);
#4276=ORIENTED_EDGE('',*,*,#3232,.F.);
#4277=ORIENTED_EDGE('',*,*,#3233,.F.);
#4278=ORIENTED_EDGE('',*,*,#3232,.T.);
#4279=ORIENTED_EDGE('',*,*,#3234,.T.);
#4280=ORIENTED_EDGE('',*,*,#3224,.T.);
#4281=ORIENTED_EDGE('',*,*,#3234,.F.);
#4282=ORIENTED_EDGE('',*,*,#3231,.T.);
#4283=ORIENTED_EDGE('',*,*,#3228,.T.);
#4284=ORIENTED_EDGE('',*,*,#3225,.T.);
#4285=ORIENTED_EDGE('',*,*,#3235,.F.);
#4286=ORIENTED_EDGE('',*,*,#3236,.T.);
#4287=ORIENTED_EDGE('',*,*,#3237,.F.);
#4288=ORIENTED_EDGE('',*,*,#3238,.T.);
#4289=ORIENTED_EDGE('',*,*,#3235,.T.);
#4290=ORIENTED_EDGE('',*,*,#3238,.F.);
#4291=ORIENTED_EDGE('',*,*,#3237,.T.);
#4292=ORIENTED_EDGE('',*,*,#3239,.F.);
#4293=ORIENTED_EDGE('',*,*,#3240,.F.);
#4294=ORIENTED_EDGE('',*,*,#3241,.T.);
#4295=ORIENTED_EDGE('',*,*,#3239,.T.);
#4296=ORIENTED_EDGE('',*,*,#3241,.F.);
#4297=ORIENTED_EDGE('',*,*,#3242,.F.);
#4298=ORIENTED_EDGE('',*,*,#3240,.T.);
#4299=ORIENTED_EDGE('',*,*,#3243,.F.);
#4300=ORIENTED_EDGE('',*,*,#3244,.T.);
#4301=ORIENTED_EDGE('',*,*,#3242,.T.);
#4302=ORIENTED_EDGE('',*,*,#3244,.F.);
#4303=ORIENTED_EDGE('',*,*,#3243,.T.);
#4304=ORIENTED_EDGE('',*,*,#3245,.F.);
#4305=ORIENTED_EDGE('',*,*,#3246,.F.);
#4306=ORIENTED_EDGE('',*,*,#3247,.T.);
#4307=ORIENTED_EDGE('',*,*,#3245,.T.);
#4308=ORIENTED_EDGE('',*,*,#3247,.F.);
#4309=ORIENTED_EDGE('',*,*,#3248,.F.);
#4310=ORIENTED_EDGE('',*,*,#3246,.T.);
#4311=ORIENTED_EDGE('',*,*,#3249,.F.);
#4312=ORIENTED_EDGE('',*,*,#3250,.T.);
#4313=ORIENTED_EDGE('',*,*,#3248,.T.);
#4314=ORIENTED_EDGE('',*,*,#3250,.F.);
#4315=ORIENTED_EDGE('',*,*,#3249,.T.);
#4316=ORIENTED_EDGE('',*,*,#3251,.F.);
#4317=ORIENTED_EDGE('',*,*,#3251,.T.);
#4318=ORIENTED_EDGE('',*,*,#3252,.T.);
#4319=ORIENTED_EDGE('',*,*,#3236,.F.);
#4320=ORIENTED_EDGE('',*,*,#3252,.F.);
#4321=ORIENTED_EDGE('',*,*,#3230,.T.);
#4322=ORIENTED_EDGE('',*,*,#3233,.T.);
#4323=ORIENTED_EDGE('',*,*,#3223,.T.);
#4324=ORIENTED_EDGE('',*,*,#3227,.T.);
#4325=ORIENTED_EDGE('',*,*,#3253,.F.);
#4326=ORIENTED_EDGE('',*,*,#3254,.F.);
#4327=ORIENTED_EDGE('',*,*,#3255,.F.);
#4328=ORIENTED_EDGE('',*,*,#3256,.F.);
#4329=ORIENTED_EDGE('',*,*,#3257,.F.);
#4330=ORIENTED_EDGE('',*,*,#3256,.T.);
#4331=ORIENTED_EDGE('',*,*,#3258,.F.);
#4332=ORIENTED_EDGE('',*,*,#3259,.T.);
#4333=ORIENTED_EDGE('',*,*,#3260,.F.);
#4334=ORIENTED_EDGE('',*,*,#3259,.F.);
#4335=ORIENTED_EDGE('',*,*,#3261,.F.);
#4336=ORIENTED_EDGE('',*,*,#3262,.F.);
#4337=ORIENTED_EDGE('',*,*,#3263,.F.);
#4338=ORIENTED_EDGE('',*,*,#3262,.T.);
#4339=ORIENTED_EDGE('',*,*,#3264,.F.);
#4340=ORIENTED_EDGE('',*,*,#3254,.T.);
#4341=ORIENTED_EDGE('',*,*,#3265,.F.);
#4342=ORIENTED_EDGE('',*,*,#3266,.T.);
#4343=ORIENTED_EDGE('',*,*,#3267,.F.);
#4344=ORIENTED_EDGE('',*,*,#3268,.T.);
#4345=ORIENTED_EDGE('',*,*,#3265,.T.);
#4346=ORIENTED_EDGE('',*,*,#3268,.F.);
#4347=ORIENTED_EDGE('',*,*,#3260,.T.);
#4348=ORIENTED_EDGE('',*,*,#3263,.T.);
#4349=ORIENTED_EDGE('',*,*,#3253,.T.);
#4350=ORIENTED_EDGE('',*,*,#3257,.T.);
#4351=ORIENTED_EDGE('',*,*,#3267,.T.);
#4352=ORIENTED_EDGE('',*,*,#3269,.F.);
#4353=ORIENTED_EDGE('',*,*,#3269,.T.);
#4354=ORIENTED_EDGE('',*,*,#3270,.T.);
#4355=ORIENTED_EDGE('',*,*,#3266,.F.);
#4356=ORIENTED_EDGE('',*,*,#3270,.F.);
#4357=ORIENTED_EDGE('',*,*,#3261,.T.);
#4358=ORIENTED_EDGE('',*,*,#3258,.T.);
#4359=ORIENTED_EDGE('',*,*,#3255,.T.);
#4360=ORIENTED_EDGE('',*,*,#3264,.T.);
#4361=ORIENTED_EDGE('',*,*,#3271,.F.);
#4362=ORIENTED_EDGE('',*,*,#3272,.T.);
#4363=ORIENTED_EDGE('',*,*,#3273,.F.);
#4364=ORIENTED_EDGE('',*,*,#3272,.F.);
#4365=ORIENTED_EDGE('',*,*,#3274,.F.);
#4366=ORIENTED_EDGE('',*,*,#3275,.T.);
#4367=ORIENTED_EDGE('',*,*,#3276,.F.);
#4368=ORIENTED_EDGE('',*,*,#3275,.F.);
#4369=ORIENTED_EDGE('',*,*,#3277,.F.);
#4370=ORIENTED_EDGE('',*,*,#3278,.T.);
#4371=ORIENTED_EDGE('',*,*,#3279,.F.);
#4372=ORIENTED_EDGE('',*,*,#3278,.F.);
#4373=ORIENTED_EDGE('',*,*,#3280,.F.);
#4374=ORIENTED_EDGE('',*,*,#3281,.T.);
#4375=ORIENTED_EDGE('',*,*,#3282,.F.);
#4376=ORIENTED_EDGE('',*,*,#3281,.F.);
#4377=ORIENTED_EDGE('',*,*,#3283,.F.);
#4378=ORIENTED_EDGE('',*,*,#3284,.T.);
#4379=ORIENTED_EDGE('',*,*,#3285,.F.);
#4380=ORIENTED_EDGE('',*,*,#3284,.F.);
#4381=ORIENTED_EDGE('',*,*,#3286,.F.);
#4382=ORIENTED_EDGE('',*,*,#3287,.T.);
#4383=ORIENTED_EDGE('',*,*,#3288,.F.);
#4384=ORIENTED_EDGE('',*,*,#3287,.F.);
#4385=ORIENTED_EDGE('',*,*,#3289,.T.);
#4386=ORIENTED_EDGE('',*,*,#3290,.T.);
#4387=ORIENTED_EDGE('',*,*,#3291,.F.);
#4388=ORIENTED_EDGE('',*,*,#3292,.F.);
#4389=ORIENTED_EDGE('',*,*,#3293,.T.);
#4390=ORIENTED_EDGE('',*,*,#3292,.T.);
#4391=ORIENTED_EDGE('',*,*,#3294,.F.);
#4392=ORIENTED_EDGE('',*,*,#3295,.F.);
#4393=ORIENTED_EDGE('',*,*,#3288,.T.);
#4394=ORIENTED_EDGE('',*,*,#3285,.T.);
#4395=ORIENTED_EDGE('',*,*,#3282,.T.);
#4396=ORIENTED_EDGE('',*,*,#3279,.T.);
#4397=ORIENTED_EDGE('',*,*,#3276,.T.);
#4398=ORIENTED_EDGE('',*,*,#3273,.T.);
#4399=ORIENTED_EDGE('',*,*,#3296,.T.);
#4400=ORIENTED_EDGE('',*,*,#3295,.T.);
#4401=ORIENTED_EDGE('',*,*,#3297,.F.);
#4402=ORIENTED_EDGE('',*,*,#3298,.F.);
#4403=ORIENTED_EDGE('',*,*,#3299,.T.);
#4404=ORIENTED_EDGE('',*,*,#3298,.T.);
#4405=ORIENTED_EDGE('',*,*,#3300,.F.);
#4406=ORIENTED_EDGE('',*,*,#3290,.F.);
#4407=ORIENTED_EDGE('',*,*,#3286,.T.);
#4408=ORIENTED_EDGE('',*,*,#3283,.T.);
#4409=ORIENTED_EDGE('',*,*,#3280,.T.);
#4410=ORIENTED_EDGE('',*,*,#3277,.T.);
#4411=ORIENTED_EDGE('',*,*,#3274,.T.);
#4412=ORIENTED_EDGE('',*,*,#3271,.T.);
#4413=ORIENTED_EDGE('',*,*,#3300,.T.);
#4414=ORIENTED_EDGE('',*,*,#3297,.T.);
#4415=ORIENTED_EDGE('',*,*,#3294,.T.);
#4416=ORIENTED_EDGE('',*,*,#3291,.T.);
#4417=ORIENTED_EDGE('',*,*,#3299,.F.);
#4418=ORIENTED_EDGE('',*,*,#3289,.F.);
#4419=ORIENTED_EDGE('',*,*,#3293,.F.);
#4420=ORIENTED_EDGE('',*,*,#3296,.F.);
#4421=ORIENTED_EDGE('',*,*,#3301,.F.);
#4422=ORIENTED_EDGE('',*,*,#3302,.F.);
#4423=ORIENTED_EDGE('',*,*,#3303,.T.);
#4424=ORIENTED_EDGE('',*,*,#3301,.T.);
#4425=ORIENTED_EDGE('',*,*,#3303,.F.);
#4426=ORIENTED_EDGE('',*,*,#3304,.F.);
#4427=ORIENTED_EDGE('',*,*,#3305,.T.);
#4428=ORIENTED_EDGE('',*,*,#3302,.T.);
#4429=ORIENTED_EDGE('',*,*,#3305,.F.);
#4430=ORIENTED_EDGE('',*,*,#3306,.F.);
#4431=ORIENTED_EDGE('',*,*,#3307,.T.);
#4432=ORIENTED_EDGE('',*,*,#3304,.T.);
#4433=ORIENTED_EDGE('',*,*,#3307,.F.);
#4434=ORIENTED_EDGE('',*,*,#3306,.T.);
#4435=ORIENTED_EDGE('',*,*,#3308,.F.);
#4436=ORIENTED_EDGE('',*,*,#3309,.F.);
#4437=ORIENTED_EDGE('',*,*,#3310,.T.);
#4438=ORIENTED_EDGE('',*,*,#3308,.T.);
#4439=ORIENTED_EDGE('',*,*,#3310,.F.);
#4440=ORIENTED_EDGE('',*,*,#3311,.F.);
#4441=ORIENTED_EDGE('',*,*,#3312,.T.);
#4442=ORIENTED_EDGE('',*,*,#3309,.T.);
#4443=ORIENTED_EDGE('',*,*,#3312,.F.);
#4444=ORIENTED_EDGE('',*,*,#3313,.F.);
#4445=ORIENTED_EDGE('',*,*,#3314,.T.);
#4446=ORIENTED_EDGE('',*,*,#3311,.T.);
#4447=ORIENTED_EDGE('',*,*,#3314,.F.);
#4448=ORIENTED_EDGE('',*,*,#3313,.T.);
#4449=ORIENTED_EDGE('',*,*,#3315,.T.);
#4450=ORIENTED_EDGE('',*,*,#3316,.T.);
#4451=ORIENTED_EDGE('',*,*,#3317,.T.);
#4452=ORIENTED_EDGE('',*,*,#3318,.F.);
#4453=ORIENTED_EDGE('',*,*,#3319,.T.);
#4454=ORIENTED_EDGE('',*,*,#3320,.T.);
#4455=ORIENTED_EDGE('',*,*,#3321,.T.);
#4456=ORIENTED_EDGE('',*,*,#3316,.F.);
#4457=ORIENTED_EDGE('',*,*,#3322,.T.);
#4458=ORIENTED_EDGE('',*,*,#3323,.T.);
#4459=ORIENTED_EDGE('',*,*,#3324,.T.);
#4460=ORIENTED_EDGE('',*,*,#3320,.F.);
#4461=ORIENTED_EDGE('',*,*,#3325,.T.);
#4462=ORIENTED_EDGE('',*,*,#3326,.T.);
#4463=ORIENTED_EDGE('',*,*,#3327,.T.);
#4464=ORIENTED_EDGE('',*,*,#3323,.F.);
#4465=ORIENTED_EDGE('',*,*,#3328,.T.);
#4466=ORIENTED_EDGE('',*,*,#3329,.T.);
#4467=ORIENTED_EDGE('',*,*,#3330,.T.);
#4468=ORIENTED_EDGE('',*,*,#3326,.F.);
#4469=ORIENTED_EDGE('',*,*,#3331,.T.);
#4470=ORIENTED_EDGE('',*,*,#3318,.T.);
#4471=ORIENTED_EDGE('',*,*,#3332,.T.);
#4472=ORIENTED_EDGE('',*,*,#3329,.F.);
#4473=ORIENTED_EDGE('',*,*,#3331,.F.);
#4474=ORIENTED_EDGE('',*,*,#3328,.F.);
#4475=ORIENTED_EDGE('',*,*,#3325,.F.);
#4476=ORIENTED_EDGE('',*,*,#3322,.F.);
#4477=ORIENTED_EDGE('',*,*,#3319,.F.);
#4478=ORIENTED_EDGE('',*,*,#3315,.F.);
#4479=ORIENTED_EDGE('',*,*,#3332,.F.);
#4480=ORIENTED_EDGE('',*,*,#3317,.F.);
#4481=ORIENTED_EDGE('',*,*,#3321,.F.);
#4482=ORIENTED_EDGE('',*,*,#3324,.F.);
#4483=ORIENTED_EDGE('',*,*,#3327,.F.);
#4484=ORIENTED_EDGE('',*,*,#3330,.F.);
#4485=ORIENTED_EDGE('',*,*,#3333,.F.);
#4486=ORIENTED_EDGE('',*,*,#3334,.F.);
#4487=ORIENTED_EDGE('',*,*,#3335,.T.);
#4488=ORIENTED_EDGE('',*,*,#3333,.T.);
#4489=ORIENTED_EDGE('',*,*,#3335,.F.);
#4490=ORIENTED_EDGE('',*,*,#3336,.F.);
#4491=ORIENTED_EDGE('',*,*,#3337,.T.);
#4492=ORIENTED_EDGE('',*,*,#3334,.T.);
#4493=ORIENTED_EDGE('',*,*,#3337,.F.);
#4494=ORIENTED_EDGE('',*,*,#3338,.F.);
#4495=ORIENTED_EDGE('',*,*,#3339,.T.);
#4496=ORIENTED_EDGE('',*,*,#3336,.T.);
#4497=ORIENTED_EDGE('',*,*,#3339,.F.);
#4498=ORIENTED_EDGE('',*,*,#3338,.T.);
#4499=ORIENTED_EDGE('',*,*,#3340,.F.);
#4500=ORIENTED_EDGE('',*,*,#3341,.F.);
#4501=ORIENTED_EDGE('',*,*,#3342,.T.);
#4502=ORIENTED_EDGE('',*,*,#3340,.T.);
#4503=ORIENTED_EDGE('',*,*,#3342,.F.);
#4504=ORIENTED_EDGE('',*,*,#3343,.F.);
#4505=ORIENTED_EDGE('',*,*,#3344,.T.);
#4506=ORIENTED_EDGE('',*,*,#3341,.T.);
#4507=ORIENTED_EDGE('',*,*,#3344,.F.);
#4508=ORIENTED_EDGE('',*,*,#3345,.F.);
#4509=ORIENTED_EDGE('',*,*,#3346,.T.);
#4510=ORIENTED_EDGE('',*,*,#3343,.T.);
#4511=ORIENTED_EDGE('',*,*,#3346,.F.);
#4512=ORIENTED_EDGE('',*,*,#3345,.T.);
#4513=ORIENTED_EDGE('',*,*,#3347,.T.);
#4514=ORIENTED_EDGE('',*,*,#3348,.T.);
#4515=ORIENTED_EDGE('',*,*,#3349,.T.);
#4516=ORIENTED_EDGE('',*,*,#3350,.F.);
#4517=ORIENTED_EDGE('',*,*,#3351,.T.);
#4518=ORIENTED_EDGE('',*,*,#3352,.T.);
#4519=ORIENTED_EDGE('',*,*,#3353,.T.);
#4520=ORIENTED_EDGE('',*,*,#3348,.F.);
#4521=ORIENTED_EDGE('',*,*,#3354,.T.);
#4522=ORIENTED_EDGE('',*,*,#3355,.T.);
#4523=ORIENTED_EDGE('',*,*,#3356,.T.);
#4524=ORIENTED_EDGE('',*,*,#3352,.F.);
#4525=ORIENTED_EDGE('',*,*,#3357,.T.);
#4526=ORIENTED_EDGE('',*,*,#3358,.T.);
#4527=ORIENTED_EDGE('',*,*,#3359,.T.);
#4528=ORIENTED_EDGE('',*,*,#3355,.F.);
#4529=ORIENTED_EDGE('',*,*,#3360,.T.);
#4530=ORIENTED_EDGE('',*,*,#3361,.T.);
#4531=ORIENTED_EDGE('',*,*,#3362,.T.);
#4532=ORIENTED_EDGE('',*,*,#3358,.F.);
#4533=ORIENTED_EDGE('',*,*,#3363,.T.);
#4534=ORIENTED_EDGE('',*,*,#3350,.T.);
#4535=ORIENTED_EDGE('',*,*,#3364,.T.);
#4536=ORIENTED_EDGE('',*,*,#3361,.F.);
#4537=ORIENTED_EDGE('',*,*,#3363,.F.);
#4538=ORIENTED_EDGE('',*,*,#3360,.F.);
#4539=ORIENTED_EDGE('',*,*,#3357,.F.);
#4540=ORIENTED_EDGE('',*,*,#3354,.F.);
#4541=ORIENTED_EDGE('',*,*,#3351,.F.);
#4542=ORIENTED_EDGE('',*,*,#3347,.F.);
#4543=ORIENTED_EDGE('',*,*,#3364,.F.);
#4544=ORIENTED_EDGE('',*,*,#3349,.F.);
#4545=ORIENTED_EDGE('',*,*,#3353,.F.);
#4546=ORIENTED_EDGE('',*,*,#3356,.F.);
#4547=ORIENTED_EDGE('',*,*,#3359,.F.);
#4548=ORIENTED_EDGE('',*,*,#3362,.F.);
#4549=ORIENTED_EDGE('',*,*,#3365,.F.);
#4550=ORIENTED_EDGE('',*,*,#3366,.T.);
#4551=ORIENTED_EDGE('',*,*,#3367,.T.);
#4552=ORIENTED_EDGE('',*,*,#3366,.F.);
#4553=ORIENTED_EDGE('',*,*,#3368,.F.);
#4554=ORIENTED_EDGE('',*,*,#3369,.T.);
#4555=ORIENTED_EDGE('',*,*,#3370,.T.);
#4556=ORIENTED_EDGE('',*,*,#3369,.F.);
#4557=ORIENTED_EDGE('',*,*,#3368,.T.);
#4558=ORIENTED_EDGE('',*,*,#3365,.T.);
#4559=ORIENTED_EDGE('',*,*,#3370,.F.);
#4560=ORIENTED_EDGE('',*,*,#3367,.F.);
#4561=ORIENTED_EDGE('',*,*,#3371,.F.);
#4562=ORIENTED_EDGE('',*,*,#3372,.T.);
#4563=ORIENTED_EDGE('',*,*,#3373,.T.);
#4564=ORIENTED_EDGE('',*,*,#3372,.F.);
#4565=ORIENTED_EDGE('',*,*,#3374,.F.);
#4566=ORIENTED_EDGE('',*,*,#3375,.T.);
#4567=ORIENTED_EDGE('',*,*,#3376,.T.);
#4568=ORIENTED_EDGE('',*,*,#3375,.F.);
#4569=ORIENTED_EDGE('',*,*,#3374,.T.);
#4570=ORIENTED_EDGE('',*,*,#3371,.T.);
#4571=ORIENTED_EDGE('',*,*,#3376,.F.);
#4572=ORIENTED_EDGE('',*,*,#3373,.F.);
#4573=ORIENTED_EDGE('',*,*,#3377,.F.);
#4574=ORIENTED_EDGE('',*,*,#3378,.F.);
#4575=ORIENTED_EDGE('',*,*,#3379,.T.);
#4576=ORIENTED_EDGE('',*,*,#3377,.T.);
#4577=ORIENTED_EDGE('',*,*,#3379,.F.);
#4578=ORIENTED_EDGE('',*,*,#3380,.F.);
#4579=ORIENTED_EDGE('',*,*,#3381,.T.);
#4580=ORIENTED_EDGE('',*,*,#3378,.T.);
#4581=ORIENTED_EDGE('',*,*,#3381,.F.);
#4582=ORIENTED_EDGE('',*,*,#3382,.F.);
#4583=ORIENTED_EDGE('',*,*,#3383,.T.);
#4584=ORIENTED_EDGE('',*,*,#3380,.T.);
#4585=ORIENTED_EDGE('',*,*,#3383,.F.);
#4586=ORIENTED_EDGE('',*,*,#3382,.T.);
#4587=ORIENTED_EDGE('',*,*,#3384,.F.);
#4588=ORIENTED_EDGE('',*,*,#3385,.F.);
#4589=ORIENTED_EDGE('',*,*,#3386,.T.);
#4590=ORIENTED_EDGE('',*,*,#3384,.T.);
#4591=ORIENTED_EDGE('',*,*,#3386,.F.);
#4592=ORIENTED_EDGE('',*,*,#3387,.F.);
#4593=ORIENTED_EDGE('',*,*,#3388,.T.);
#4594=ORIENTED_EDGE('',*,*,#3385,.T.);
#4595=ORIENTED_EDGE('',*,*,#3388,.F.);
#4596=ORIENTED_EDGE('',*,*,#3389,.F.);
#4597=ORIENTED_EDGE('',*,*,#3390,.T.);
#4598=ORIENTED_EDGE('',*,*,#3387,.T.);
#4599=ORIENTED_EDGE('',*,*,#3390,.F.);
#4600=ORIENTED_EDGE('',*,*,#3389,.T.);
#4601=ORIENTED_EDGE('',*,*,#3391,.T.);
#4602=ORIENTED_EDGE('',*,*,#3392,.T.);
#4603=ORIENTED_EDGE('',*,*,#3393,.T.);
#4604=ORIENTED_EDGE('',*,*,#3394,.F.);
#4605=ORIENTED_EDGE('',*,*,#3395,.T.);
#4606=ORIENTED_EDGE('',*,*,#3396,.T.);
#4607=ORIENTED_EDGE('',*,*,#3397,.T.);
#4608=ORIENTED_EDGE('',*,*,#3392,.F.);
#4609=ORIENTED_EDGE('',*,*,#3398,.T.);
#4610=ORIENTED_EDGE('',*,*,#3399,.T.);
#4611=ORIENTED_EDGE('',*,*,#3400,.T.);
#4612=ORIENTED_EDGE('',*,*,#3396,.F.);
#4613=ORIENTED_EDGE('',*,*,#3401,.T.);
#4614=ORIENTED_EDGE('',*,*,#3402,.T.);
#4615=ORIENTED_EDGE('',*,*,#3403,.T.);
#4616=ORIENTED_EDGE('',*,*,#3399,.F.);
#4617=ORIENTED_EDGE('',*,*,#3404,.T.);
#4618=ORIENTED_EDGE('',*,*,#3405,.T.);
#4619=ORIENTED_EDGE('',*,*,#3406,.T.);
#4620=ORIENTED_EDGE('',*,*,#3402,.F.);
#4621=ORIENTED_EDGE('',*,*,#3407,.T.);
#4622=ORIENTED_EDGE('',*,*,#3394,.T.);
#4623=ORIENTED_EDGE('',*,*,#3408,.T.);
#4624=ORIENTED_EDGE('',*,*,#3405,.F.);
#4625=ORIENTED_EDGE('',*,*,#3407,.F.);
#4626=ORIENTED_EDGE('',*,*,#3404,.F.);
#4627=ORIENTED_EDGE('',*,*,#3401,.F.);
#4628=ORIENTED_EDGE('',*,*,#3398,.F.);
#4629=ORIENTED_EDGE('',*,*,#3395,.F.);
#4630=ORIENTED_EDGE('',*,*,#3391,.F.);
#4631=ORIENTED_EDGE('',*,*,#3408,.F.);
#4632=ORIENTED_EDGE('',*,*,#3393,.F.);
#4633=ORIENTED_EDGE('',*,*,#3397,.F.);
#4634=ORIENTED_EDGE('',*,*,#3400,.F.);
#4635=ORIENTED_EDGE('',*,*,#3403,.F.);
#4636=ORIENTED_EDGE('',*,*,#3406,.F.);
#4637=CYLINDRICAL_SURFACE('',#5292,0.210000000000001);
#4638=CYLINDRICAL_SURFACE('',#5295,0.210000000000001);
#4639=CYLINDRICAL_SURFACE('',#5298,0.210000000000001);
#4640=CYLINDRICAL_SURFACE('',#5301,0.210000000000001);
#4641=CYLINDRICAL_SURFACE('',#5304,0.210000000000001);
#4642=CYLINDRICAL_SURFACE('',#5307,0.21);
#4643=CYLINDRICAL_SURFACE('',#5310,0.21);
#4644=CYLINDRICAL_SURFACE('',#5313,0.210000000000001);
#4645=CYLINDRICAL_SURFACE('',#5316,0.210000000000001);
#4646=CYLINDRICAL_SURFACE('',#5319,0.210000000000001);
#4647=CYLINDRICAL_SURFACE('',#5322,0.21);
#4648=CYLINDRICAL_SURFACE('',#5325,0.21);
#4649=CYLINDRICAL_SURFACE('',#5328,0.21);
#4650=CYLINDRICAL_SURFACE('',#5331,0.21);
#4651=CYLINDRICAL_SURFACE('',#5334,0.210000000000001);
#4652=CYLINDRICAL_SURFACE('',#5337,0.210000000000001);
#4653=CYLINDRICAL_SURFACE('',#5350,0.6);
#4654=CYLINDRICAL_SURFACE('',#5359,0.525);
#4655=CYLINDRICAL_SURFACE('',#5361,0.525);
#4656=CYLINDRICAL_SURFACE('',#5371,0.225);
#4657=CYLINDRICAL_SURFACE('',#5374,0.165);
#4658=CYLINDRICAL_SURFACE('',#5376,0.275);
#4659=CYLINDRICAL_SURFACE('',#5378,0.275);
#4660=CYLINDRICAL_SURFACE('',#5380,0.6);
#4661=CYLINDRICAL_SURFACE('',#5409,0.425);
#4662=CYLINDRICAL_SURFACE('',#5417,0.24505);
#4663=CYLINDRICAL_SURFACE('',#5419,0.475);
#4664=CYLINDRICAL_SURFACE('',#5424,0.475);
#4665=CYLINDRICAL_SURFACE('',#5429,0.275);
#4666=CYLINDRICAL_SURFACE('',#5431,0.275);
#4667=CYLINDRICAL_SURFACE('',#5447,0.34);
#4668=CYLINDRICAL_SURFACE('',#5450,0.275);
#4669=CYLINDRICAL_SURFACE('',#5453,0.275);
#4670=CYLINDRICAL_SURFACE('',#5456,0.275);
#4671=CYLINDRICAL_SURFACE('',#5459,0.275);
#4672=CYLINDRICAL_SURFACE('',#5488,0.425);
#4673=CYLINDRICAL_SURFACE('',#5496,0.24505);
#4674=CYLINDRICAL_SURFACE('',#5498,0.3933);
#4675=CYLINDRICAL_SURFACE('',#5522,0.338975);
#4676=CYLINDRICAL_SURFACE('',#5538,0.21);
#4677=CYLINDRICAL_SURFACE('',#5542,0.605);
#4678=CYLINDRICAL_SURFACE('',#5545,1.1);
#4679=CYLINDRICAL_SURFACE('',#5562,0.24505);
#4680=CYLINDRICAL_SURFACE('',#5569,0.165);
#4681=CYLINDRICAL_SURFACE('',#5572,0.165);
#4682=CYLINDRICAL_SURFACE('',#5575,0.165);
#4683=CYLINDRICAL_SURFACE('',#5578,0.165);
#4684=CYLINDRICAL_SURFACE('',#5581,0.210000000000001);
#4685=CYLINDRICAL_SURFACE('',#5585,0.210000000000001);
#4686=CYLINDRICAL_SURFACE('',#5589,0.210000000000001);
#4687=CYLINDRICAL_SURFACE('',#5593,0.210000000000001);
#4688=CYLINDRICAL_SURFACE('',#5597,1.05);
#4689=CYLINDRICAL_SURFACE('',#5600,1.05);
#4690=CYLINDRICAL_SURFACE('',#5610,0.25);
#4691=CYLINDRICAL_SURFACE('',#5613,0.274999999999999);
#4692=CYLINDRICAL_SURFACE('',#5616,0.275);
#4693=CYLINDRICAL_SURFACE('',#5619,0.275);
#4694=CYLINDRICAL_SURFACE('',#5622,0.274999999999999);
#4695=CYLINDRICAL_SURFACE('',#5643,1.05);
#4696=CYLINDRICAL_SURFACE('',#5647,1.);
#4697=CYLINDRICAL_SURFACE('',#5651,1.05);
#4698=CYLINDRICAL_SURFACE('',#5655,1.);
#4699=CYLINDRICAL_SURFACE('',#5659,1.05);
#4700=CYLINDRICAL_SURFACE('',#5663,0.9);
#4701=CYLINDRICAL_SURFACE('',#5676,0.895);
#4702=CYLINDRICAL_SURFACE('',#5680,0.605);
#4703=CYLINDRICAL_SURFACE('',#5684,0.225);
#4704=CYLINDRICAL_SURFACE('',#5687,0.225);
#4705=CYLINDRICAL_SURFACE('',#5690,0.225);
#4706=CYLINDRICAL_SURFACE('',#5693,0.225);
#4707=CYLINDRICAL_SURFACE('',#5696,0.7);
#4708=CYLINDRICAL_SURFACE('',#5699,0.7);
#4709=CYLINDRICAL_SURFACE('',#5713,0.35);
#4710=CYLINDRICAL_SURFACE('',#5721,0.1954);
#4711=CYLINDRICAL_SURFACE('',#5739,0.425);
#4712=CYLINDRICAL_SURFACE('',#5747,0.24505);
#4713=CYLINDRICAL_SURFACE('',#5798,0.33);
#4714=CYLINDRICAL_SURFACE('',#5801,1.5);
#4715=CYLINDRICAL_SURFACE('',#5807,0.32);
#4716=CYLINDRICAL_SURFACE('',#5810,0.6);
#4717=CYLINDRICAL_SURFACE('',#5820,0.5);
#4718=CYLINDRICAL_SURFACE('',#5828,0.2942);
#4719=ADVANCED_FACE('',(#710),#4637,.F.);
#4720=ADVANCED_FACE('',(#711),#4638,.F.);
#4721=ADVANCED_FACE('',(#712),#4639,.F.);
#4722=ADVANCED_FACE('',(#713),#4640,.F.);
#4723=ADVANCED_FACE('',(#714),#4641,.F.);
#4724=ADVANCED_FACE('',(#715),#4642,.F.);
#4725=ADVANCED_FACE('',(#716),#4643,.F.);
#4726=ADVANCED_FACE('',(#717),#4644,.F.);
#4727=ADVANCED_FACE('',(#718),#4645,.F.);
#4728=ADVANCED_FACE('',(#719),#4646,.F.);
#4729=ADVANCED_FACE('',(#720),#4647,.F.);
#4730=ADVANCED_FACE('',(#721),#4648,.F.);
#4731=ADVANCED_FACE('',(#722),#4649,.F.);
#4732=ADVANCED_FACE('',(#723),#4650,.F.);
#4733=ADVANCED_FACE('',(#724),#4651,.F.);
#4734=ADVANCED_FACE('',(#725),#4652,.F.);
#4735=ADVANCED_FACE('',(#726),#531,.T.);
#4736=ADVANCED_FACE('',(#727),#532,.T.);
#4737=ADVANCED_FACE('',(#728),#533,.T.);
#4738=ADVANCED_FACE('',(#729),#534,.T.);
#4739=ADVANCED_FACE('',(#730,#406,#407,#408,#409,#410,#411,#412,#413,#414,
#415,#416,#417,#418,#419,#420,#421),#535,.T.);
#4740=ADVANCED_FACE('',(#731,#422,#423,#424,#425,#426,#427,#428,#429,#430,
#431,#432,#433,#434,#435,#436,#437),#536,.F.);
#4741=ADVANCED_FACE('',(#732),#293,.T.);
#4742=ADVANCED_FACE('',(#733),#4653,.T.);
#4743=ADVANCED_FACE('',(#734),#537,.F.);
#4744=ADVANCED_FACE('',(#735),#294,.T.);
#4745=ADVANCED_FACE('',(#736),#538,.T.);
#4746=ADVANCED_FACE('',(#737),#539,.F.);
#4747=ADVANCED_FACE('',(#738),#4654,.F.);
#4748=ADVANCED_FACE('',(#739),#4655,.F.);
#4749=ADVANCED_FACE('',(#740),#540,.F.);
#4750=ADVANCED_FACE('',(#741,#438),#541,.T.);
#4751=ADVANCED_FACE('',(#742,#439),#542,.T.);
#4752=ADVANCED_FACE('',(#743,#440),#543,.T.);
#4753=ADVANCED_FACE('',(#744),#4656,.F.);
#4754=ADVANCED_FACE('',(#745),#4657,.F.);
#4755=ADVANCED_FACE('',(#746),#4658,.F.);
#4756=ADVANCED_FACE('',(#747),#4659,.F.);
#4757=ADVANCED_FACE('',(#748),#4660,.F.);
#4758=ADVANCED_FACE('',(#749,#441),#544,.T.);
#4759=ADVANCED_FACE('',(#750),#545,.T.);
#4760=ADVANCED_FACE('',(#751,#442,#443),#546,.T.);
#4761=ADVANCED_FACE('',(#752),#547,.T.);
#4762=ADVANCED_FACE('',(#753,#444),#548,.T.);
#4763=ADVANCED_FACE('',(#754),#549,.T.);
#4764=ADVANCED_FACE('',(#755,#445),#550,.T.);
#4765=ADVANCED_FACE('',(#756),#551,.T.);
#4766=ADVANCED_FACE('',(#757,#446),#552,.T.);
#4767=ADVANCED_FACE('',(#758),#553,.T.);
#4768=ADVANCED_FACE('',(#759,#447),#554,.T.);
#4769=ADVANCED_FACE('',(#760),#555,.F.);
#4770=ADVANCED_FACE('',(#761),#556,.F.);
#4771=ADVANCED_FACE('',(#762),#557,.F.);
#4772=ADVANCED_FACE('',(#763),#558,.F.);
#4773=ADVANCED_FACE('',(#764),#559,.F.);
#4774=ADVANCED_FACE('',(#765),#560,.F.);
#4775=ADVANCED_FACE('',(#766),#561,.F.);
#4776=ADVANCED_FACE('',(#767),#562,.F.);
#4777=ADVANCED_FACE('',(#768),#563,.F.);
#4778=ADVANCED_FACE('',(#769),#564,.T.);
#4779=ADVANCED_FACE('',(#770),#295,.T.);
#4780=ADVANCED_FACE('',(#771),#4661,.T.);
#4781=ADVANCED_FACE('',(#772),#296,.T.);
#4782=ADVANCED_FACE('',(#773,#448),#565,.T.);
#4783=ADVANCED_FACE('',(#774),#297,.T.);
#4784=ADVANCED_FACE('',(#775),#4662,.T.);
#4785=ADVANCED_FACE('',(#776),#4663,.F.);
#4786=ADVANCED_FACE('',(#777,#449),#566,.T.);
#4787=ADVANCED_FACE('',(#778),#4664,.F.);
#4788=ADVANCED_FACE('',(#779,#450),#567,.T.);
#4789=ADVANCED_FACE('',(#780),#4665,.F.);
#4790=ADVANCED_FACE('',(#781),#4666,.F.);
#4791=ADVANCED_FACE('',(#782),#568,.T.);
#4792=ADVANCED_FACE('',(#783),#569,.T.);
#4793=ADVANCED_FACE('',(#784),#570,.T.);
#4794=ADVANCED_FACE('',(#785),#571,.T.);
#4795=ADVANCED_FACE('',(#786,#451,#452),#572,.T.);
#4796=ADVANCED_FACE('',(#787,#453,#454),#573,.F.);
#4797=ADVANCED_FACE('',(#788),#574,.T.);
#4798=ADVANCED_FACE('',(#789),#575,.T.);
#4799=ADVANCED_FACE('',(#790),#576,.T.);
#4800=ADVANCED_FACE('',(#791),#577,.T.);
#4801=ADVANCED_FACE('',(#792),#578,.T.);
#4802=ADVANCED_FACE('',(#793),#579,.F.);
#4803=ADVANCED_FACE('',(#794),#4667,.F.);
#4804=ADVANCED_FACE('',(#795),#4668,.F.);
#4805=ADVANCED_FACE('',(#796),#4669,.F.);
#4806=ADVANCED_FACE('',(#797),#4670,.F.);
#4807=ADVANCED_FACE('',(#798),#4671,.F.);
#4808=ADVANCED_FACE('',(#799),#580,.T.);
#4809=ADVANCED_FACE('',(#800),#581,.T.);
#4810=ADVANCED_FACE('',(#801),#582,.T.);
#4811=ADVANCED_FACE('',(#802,#455),#583,.T.);
#4812=ADVANCED_FACE('',(#803,#456),#584,.F.);
#4813=ADVANCED_FACE('',(#804),#585,.T.);
#4814=ADVANCED_FACE('',(#805),#586,.T.);
#4815=ADVANCED_FACE('',(#806),#587,.T.);
#4816=ADVANCED_FACE('',(#807),#588,.T.);
#4817=ADVANCED_FACE('',(#808,#457,#458,#459,#460,#461),#589,.T.);
#4818=ADVANCED_FACE('',(#809,#462,#463,#464,#465),#590,.F.);
#4819=ADVANCED_FACE('',(#810),#591,.F.);
#4820=ADVANCED_FACE('',(#811),#592,.F.);
#4821=ADVANCED_FACE('',(#812),#593,.F.);
#4822=ADVANCED_FACE('',(#813),#594,.F.);
#4823=ADVANCED_FACE('',(#814),#595,.F.);
#4824=ADVANCED_FACE('',(#815),#596,.F.);
#4825=ADVANCED_FACE('',(#816),#597,.F.);
#4826=ADVANCED_FACE('',(#817),#598,.F.);
#4827=ADVANCED_FACE('',(#818),#599,.F.);
#4828=ADVANCED_FACE('',(#819),#600,.T.);
#4829=ADVANCED_FACE('',(#820),#298,.T.);
#4830=ADVANCED_FACE('',(#821),#4672,.T.);
#4831=ADVANCED_FACE('',(#822),#299,.T.);
#4832=ADVANCED_FACE('',(#823,#466),#601,.T.);
#4833=ADVANCED_FACE('',(#824),#300,.T.);
#4834=ADVANCED_FACE('',(#825),#4673,.T.);
#4835=ADVANCED_FACE('',(#826),#4674,.T.);
#4836=ADVANCED_FACE('',(#827),#301,.T.);
#4837=ADVANCED_FACE('',(#828),#602,.T.);
#4838=ADVANCED_FACE('',(#829),#302,.T.);
#4839=ADVANCED_FACE('',(#830),#603,.T.);
#4840=ADVANCED_FACE('',(#831),#604,.T.);
#4841=ADVANCED_FACE('',(#832),#605,.T.);
#4842=ADVANCED_FACE('',(#833),#606,.T.);
#4843=ADVANCED_FACE('',(#834),#607,.T.);
#4844=ADVANCED_FACE('',(#835),#608,.T.);
#4845=ADVANCED_FACE('',(#836),#609,.T.);
#4846=ADVANCED_FACE('',(#837,#467),#610,.F.);
#4847=ADVANCED_FACE('',(#838),#303,.T.);
#4848=ADVANCED_FACE('',(#839),#304,.T.);
#4849=ADVANCED_FACE('',(#840),#611,.T.);
#4850=ADVANCED_FACE('',(#841),#612,.T.);
#4851=ADVANCED_FACE('',(#842),#613,.T.);
#4852=ADVANCED_FACE('',(#843),#4675,.F.);
#4853=ADVANCED_FACE('',(#844),#614,.T.);
#4854=ADVANCED_FACE('',(#845),#615,.T.);
#4855=ADVANCED_FACE('',(#846),#616,.T.);
#4856=ADVANCED_FACE('',(#847,#468),#617,.T.);
#4857=ADVANCED_FACE('',(#848,#469),#618,.F.);
#4858=ADVANCED_FACE('',(#849),#264,.T.);
#4859=ADVANCED_FACE('',(#850),#619,.T.);
#4860=ADVANCED_FACE('',(#851),#620,.F.);
#4861=ADVANCED_FACE('',(#852),#621,.T.);
#4862=ADVANCED_FACE('',(#853),#4676,.F.);
#4863=ADVANCED_FACE('',(#854),#622,.T.);
#4864=ADVANCED_FACE('',(#855,#470),#4677,.F.);
#4865=ADVANCED_FACE('',(#856,#471),#4678,.T.);
#4866=ADVANCED_FACE('',(#857,#472),#623,.T.);
#4867=ADVANCED_FACE('',(#858,#473),#624,.F.);
#4868=ADVANCED_FACE('',(#859),#625,.F.);
#4869=ADVANCED_FACE('',(#860),#626,.F.);
#4870=ADVANCED_FACE('',(#861),#627,.F.);
#4871=ADVANCED_FACE('',(#862),#628,.F.);
#4872=ADVANCED_FACE('',(#863),#629,.F.);
#4873=ADVANCED_FACE('',(#864),#630,.F.);
#4874=ADVANCED_FACE('',(#865),#631,.F.);
#4875=ADVANCED_FACE('',(#866,#474),#632,.T.);
#4876=ADVANCED_FACE('',(#867),#305,.T.);
#4877=ADVANCED_FACE('',(#868),#4679,.T.);
#4878=ADVANCED_FACE('',(#869),#306,.T.);
#4879=ADVANCED_FACE('',(#870),#633,.T.);
#4880=ADVANCED_FACE('',(#871),#4680,.F.);
#4881=ADVANCED_FACE('',(#872),#4681,.F.);
#4882=ADVANCED_FACE('',(#873),#4682,.F.);
#4883=ADVANCED_FACE('',(#874),#4683,.F.);
#4884=ADVANCED_FACE('',(#875),#4684,.F.);
#4885=ADVANCED_FACE('',(#876),#634,.T.);
#4886=ADVANCED_FACE('',(#877),#4685,.F.);
#4887=ADVANCED_FACE('',(#878),#635,.T.);
#4888=ADVANCED_FACE('',(#879),#4686,.F.);
#4889=ADVANCED_FACE('',(#880),#636,.T.);
#4890=ADVANCED_FACE('',(#881),#4687,.F.);
#4891=ADVANCED_FACE('',(#882),#637,.T.);
#4892=ADVANCED_FACE('',(#883),#4688,.F.);
#4893=ADVANCED_FACE('',(#884),#4689,.F.);
#4894=ADVANCED_FACE('',(#885),#638,.T.);
#4895=ADVANCED_FACE('',(#886,#475,#476,#477,#478,#479,#480),#639,.T.);
#4896=ADVANCED_FACE('',(#887),#640,.T.);
#4897=ADVANCED_FACE('',(#888,#481,#482,#483,#484,#485,#486),#641,.T.);
#4898=ADVANCED_FACE('',(#889,#487,#488,#489,#490),#642,.T.);
#4899=ADVANCED_FACE('',(#890),#643,.F.);
#4900=ADVANCED_FACE('',(#891),#4690,.F.);
#4901=ADVANCED_FACE('',(#892),#4691,.F.);
#4902=ADVANCED_FACE('',(#893),#4692,.F.);
#4903=ADVANCED_FACE('',(#894),#4693,.F.);
#4904=ADVANCED_FACE('',(#895),#4694,.F.);
#4905=ADVANCED_FACE('',(#896),#644,.T.);
#4906=ADVANCED_FACE('',(#897),#645,.T.);
#4907=ADVANCED_FACE('',(#898),#646,.T.);
#4908=ADVANCED_FACE('',(#899),#647,.T.);
#4909=ADVANCED_FACE('',(#900,#491,#492,#493,#494,#495),#648,.T.);
#4910=ADVANCED_FACE('',(#901,#496,#497,#498,#499,#500),#649,.F.);
#4911=ADVANCED_FACE('',(#902),#650,.F.);
#4912=ADVANCED_FACE('',(#903),#651,.F.);
#4913=ADVANCED_FACE('',(#904),#652,.F.);
#4914=ADVANCED_FACE('',(#905),#653,.F.);
#4915=ADVANCED_FACE('',(#906),#654,.F.);
#4916=ADVANCED_FACE('',(#907,#501),#655,.T.);
#4917=ADVANCED_FACE('',(#908),#4695,.T.);
#4918=ADVANCED_FACE('',(#909,#502),#656,.T.);
#4919=ADVANCED_FACE('',(#910),#4696,.T.);
#4920=ADVANCED_FACE('',(#911,#503),#657,.T.);
#4921=ADVANCED_FACE('',(#912),#4697,.T.);
#4922=ADVANCED_FACE('',(#913,#504),#658,.T.);
#4923=ADVANCED_FACE('',(#914),#4698,.T.);
#4924=ADVANCED_FACE('',(#915,#505),#659,.T.);
#4925=ADVANCED_FACE('',(#916),#4699,.T.);
#4926=ADVANCED_FACE('',(#917,#506),#660,.T.);
#4927=ADVANCED_FACE('',(#918,#507),#4700,.F.);
#4928=ADVANCED_FACE('',(#919),#661,.F.);
#4929=ADVANCED_FACE('',(#920),#662,.F.);
#4930=ADVANCED_FACE('',(#921),#663,.F.);
#4931=ADVANCED_FACE('',(#922),#664,.F.);
#4932=ADVANCED_FACE('',(#923,#508),#665,.T.);
#4933=ADVANCED_FACE('',(#924,#509),#4701,.T.);
#4934=ADVANCED_FACE('',(#925,#510),#666,.T.);
#4935=ADVANCED_FACE('',(#926,#511),#4702,.F.);
#4936=ADVANCED_FACE('',(#927),#4703,.F.);
#4937=ADVANCED_FACE('',(#928),#4704,.F.);
#4938=ADVANCED_FACE('',(#929),#4705,.F.);
#4939=ADVANCED_FACE('',(#930),#4706,.F.);
#4940=ADVANCED_FACE('',(#931),#4707,.F.);
#4941=ADVANCED_FACE('',(#932),#4708,.F.);
#4942=ADVANCED_FACE('',(#933),#667,.T.);
#4943=ADVANCED_FACE('',(#934,#512,#513,#514,#515,#516,#517),#668,.T.);
#4944=ADVANCED_FACE('',(#935),#669,.T.);
#4945=ADVANCED_FACE('',(#936,#518,#519,#520,#521,#522,#523),#670,.T.);
#4946=ADVANCED_FACE('',(#937),#671,.T.);
#4947=ADVANCED_FACE('',(#938),#672,.F.);
#4948=ADVANCED_FACE('',(#939),#673,.T.);
#4949=ADVANCED_FACE('',(#940),#307,.T.);
#4950=ADVANCED_FACE('',(#941),#4709,.T.);
#4951=ADVANCED_FACE('',(#942),#308,.T.);
#4952=ADVANCED_FACE('',(#943,#524),#674,.T.);
#4953=ADVANCED_FACE('',(#944),#309,.T.);
#4954=ADVANCED_FACE('',(#945),#4710,.T.);
#4955=ADVANCED_FACE('',(#946),#310,.T.);
#4956=ADVANCED_FACE('',(#947),#675,.T.);
#4957=ADVANCED_FACE('',(#948),#676,.F.);
#4958=ADVANCED_FACE('',(#949),#677,.F.);
#4959=ADVANCED_FACE('',(#950),#678,.F.);
#4960=ADVANCED_FACE('',(#951),#679,.F.);
#4961=ADVANCED_FACE('',(#952),#680,.F.);
#4962=ADVANCED_FACE('',(#953),#681,.F.);
#4963=ADVANCED_FACE('',(#954),#682,.F.);
#4964=ADVANCED_FACE('',(#955),#683,.F.);
#4965=ADVANCED_FACE('',(#956),#684,.T.);
#4966=ADVANCED_FACE('',(#957),#311,.T.);
#4967=ADVANCED_FACE('',(#958),#4711,.T.);
#4968=ADVANCED_FACE('',(#959),#312,.T.);
#4969=ADVANCED_FACE('',(#960,#525),#685,.T.);
#4970=ADVANCED_FACE('',(#961),#313,.T.);
#4971=ADVANCED_FACE('',(#962),#4712,.T.);
#4972=ADVANCED_FACE('',(#963),#314,.T.);
#4973=ADVANCED_FACE('',(#964),#686,.T.);
#4974=ADVANCED_FACE('',(#965),#687,.F.);
#4975=ADVANCED_FACE('',(#966),#688,.F.);
#4976=ADVANCED_FACE('',(#967),#689,.F.);
#4977=ADVANCED_FACE('',(#968),#690,.F.);
#4978=ADVANCED_FACE('',(#969),#691,.F.);
#4979=ADVANCED_FACE('',(#970),#692,.F.);
#4980=ADVANCED_FACE('',(#971),#693,.F.);
#4981=ADVANCED_FACE('',(#972),#694,.F.);
#4982=ADVANCED_FACE('',(#973),#4713,.F.);
#4983=ADVANCED_FACE('',(#974),#4714,.T.);
#4984=ADVANCED_FACE('',(#975,#526),#695,.T.);
#4985=ADVANCED_FACE('',(#976,#527),#696,.F.);
#4986=ADVANCED_FACE('',(#977),#4715,.F.);
#4987=ADVANCED_FACE('',(#978),#4716,.T.);
#4988=ADVANCED_FACE('',(#979,#528),#697,.T.);
#4989=ADVANCED_FACE('',(#980,#529),#698,.F.);
#4990=ADVANCED_FACE('',(#981),#699,.T.);
#4991=ADVANCED_FACE('',(#982),#315,.T.);
#4992=ADVANCED_FACE('',(#983),#4717,.T.);
#4993=ADVANCED_FACE('',(#984),#316,.T.);
#4994=ADVANCED_FACE('',(#985,#530),#700,.T.);
#4995=ADVANCED_FACE('',(#986),#317,.T.);
#4996=ADVANCED_FACE('',(#987),#4718,.T.);
#4997=ADVANCED_FACE('',(#988),#318,.T.);
#4998=ADVANCED_FACE('',(#989),#701,.T.);
#4999=ADVANCED_FACE('',(#990),#702,.F.);
#5000=ADVANCED_FACE('',(#991),#703,.F.);
#5001=ADVANCED_FACE('',(#992),#704,.F.);
#5002=ADVANCED_FACE('',(#993),#705,.F.);
#5003=ADVANCED_FACE('',(#994),#706,.F.);
#5004=ADVANCED_FACE('',(#995),#707,.F.);
#5005=ADVANCED_FACE('',(#996),#708,.F.);
#5006=ADVANCED_FACE('',(#997),#709,.F.);
#5007=CLOSED_SHELL('',(#4719,#4720,#4721,#4722,#4723,#4724,#4725,#4726,
#4727,#4728,#4729,#4730,#4731,#4732,#4733,#4734,#4735,#4736,#4737,#4738,
#4739,#4740));
#5008=CLOSED_SHELL('',(#4741,#4742,#4743,#4744,#4745));
#5009=CLOSED_SHELL('',(#4746,#4747,#4748,#4749,#4750,#4751,#4752,#4753,
#4754,#4755,#4756,#4757,#4758,#4759,#4760,#4761,#4762,#4763,#4764,#4765,
#4766,#4767,#4768));
#5010=CLOSED_SHELL('',(#4769,#4770,#4771,#4772,#4773,#4774,#4775,#4776));
#5011=CLOSED_SHELL('',(#4777,#4778,#4779,#4780,#4781,#4782,#4783,#4784));
#5012=CLOSED_SHELL('',(#4785,#4786,#4787,#4788,#4789,#4790,#4791,#4792,
#4793,#4794,#4795,#4796));
#5013=CLOSED_SHELL('',(#4797,#4798,#4799,#4800,#4801,#4802));
#5014=CLOSED_SHELL('',(#4803,#4804,#4805,#4806,#4807,#4808,#4809,#4810,
#4811,#4812,#4813,#4814,#4815,#4816,#4817,#4818));
#5015=CLOSED_SHELL('',(#4819,#4820,#4821,#4822,#4823,#4824,#4825,#4826));
#5016=CLOSED_SHELL('',(#4827,#4828,#4829,#4830,#4831,#4832,#4833,#4834));
#5017=CLOSED_SHELL('',(#4835,#4836,#4837,#4838,#4839,#4840,#4841,#4842,
#4843,#4844,#4845,#4846));
#5018=CLOSED_SHELL('',(#4847,#4848,#4849,#4850,#4851,#4852,#4853,#4854,
#4855,#4856,#4857));
#5019=CLOSED_SHELL('',(#4858,#4859,#4860));
#5020=CLOSED_SHELL('',(#4861,#4862,#4863,#4864,#4865,#4866,#4867));
#5021=CLOSED_SHELL('',(#4868,#4869,#4870,#4871,#4872,#4873,#4874,#4875,
#4876,#4877,#4878,#4879));
#5022=CLOSED_SHELL('',(#4880,#4881,#4882,#4883,#4884,#4885,#4886,#4887,
#4888,#4889,#4890,#4891,#4892,#4893,#4894,#4895,#4896,#4897,#4898,#4899));
#5023=CLOSED_SHELL('',(#4900,#4901,#4902,#4903,#4904,#4905,#4906,#4907,
#4908,#4909,#4910));
#5024=CLOSED_SHELL('',(#4911,#4912,#4913,#4914,#4915,#4916,#4917,#4918,
#4919,#4920,#4921,#4922,#4923,#4924,#4925,#4926,#4927));
#5025=CLOSED_SHELL('',(#4928,#4929,#4930,#4931,#4932,#4933,#4934,#4935));
#5026=CLOSED_SHELL('',(#4936,#4937,#4938,#4939,#4940,#4941,#4942,#4943,
#4944,#4945,#4946,#4947));
#5027=CLOSED_SHELL('',(#4948,#4949,#4950,#4951,#4952,#4953,#4954,#4955,
#4956));
#5028=CLOSED_SHELL('',(#4957,#4958,#4959,#4960,#4961,#4962,#4963,#4964));
#5029=CLOSED_SHELL('',(#4965,#4966,#4967,#4968,#4969,#4970,#4971,#4972,
#4973));
#5030=CLOSED_SHELL('',(#4974,#4975,#4976,#4977,#4978,#4979,#4980,#4981));
#5031=CLOSED_SHELL('',(#4982,#4983,#4984,#4985));
#5032=CLOSED_SHELL('',(#4986,#4987,#4988,#4989));
#5033=CLOSED_SHELL('',(#4990,#4991,#4992,#4993,#4994,#4995,#4996,#4997,
#4998));
#5034=CLOSED_SHELL('',(#4999,#5000,#5001,#5002,#5003,#5004,#5005,#5006));
#5035=DERIVED_UNIT_ELEMENT(#5081,1.);
#5036=DERIVED_UNIT_ELEMENT(#10294,-3.);
#5037=DERIVED_UNIT_ELEMENT(#5081,1.);
#5038=DERIVED_UNIT_ELEMENT(#10294,-3.);
#5039=DERIVED_UNIT_ELEMENT(#5081,1.);
#5040=DERIVED_UNIT_ELEMENT(#10294,-3.);
#5041=DERIVED_UNIT_ELEMENT(#5081,1.);
#5042=DERIVED_UNIT_ELEMENT(#10294,-3.);
#5043=DERIVED_UNIT_ELEMENT(#5081,1.);
#5044=DERIVED_UNIT_ELEMENT(#10294,-3.);
#5045=DERIVED_UNIT_ELEMENT(#5081,1.);
#5046=DERIVED_UNIT_ELEMENT(#10294,-3.);
#5047=DERIVED_UNIT_ELEMENT(#5081,1.);
#5048=DERIVED_UNIT_ELEMENT(#10294,-3.);
#5049=DERIVED_UNIT_ELEMENT(#5081,1.);
#5050=DERIVED_UNIT_ELEMENT(#10294,-3.);
#5051=DERIVED_UNIT_ELEMENT(#5081,1.);
#5052=DERIVED_UNIT_ELEMENT(#10294,-3.);
#5053=DERIVED_UNIT_ELEMENT(#5081,1.);
#5054=DERIVED_UNIT_ELEMENT(#10294,-3.);
#5055=DERIVED_UNIT_ELEMENT(#5081,1.);
#5056=DERIVED_UNIT_ELEMENT(#10294,-3.);
#5057=DERIVED_UNIT_ELEMENT(#5081,1.);
#5058=DERIVED_UNIT_ELEMENT(#10294,-3.);
#5059=DERIVED_UNIT_ELEMENT(#5081,1.);
#5060=DERIVED_UNIT_ELEMENT(#10294,-3.);
#5061=DERIVED_UNIT_ELEMENT(#5081,1.);
#5062=DERIVED_UNIT_ELEMENT(#10294,-3.);
#5063=DERIVED_UNIT_ELEMENT(#5081,1.);
#5064=DERIVED_UNIT_ELEMENT(#10294,-3.);
#5065=DERIVED_UNIT_ELEMENT(#5081,1.);
#5066=DERIVED_UNIT_ELEMENT(#10294,-3.);
#5067=DERIVED_UNIT_ELEMENT(#5081,1.);
#5068=DERIVED_UNIT_ELEMENT(#10294,-3.);
#5069=DERIVED_UNIT_ELEMENT(#5081,1.);
#5070=DERIVED_UNIT_ELEMENT(#10294,-3.);
#5071=DERIVED_UNIT_ELEMENT(#5081,1.);
#5072=DERIVED_UNIT_ELEMENT(#10294,-3.);
#5073=DERIVED_UNIT_ELEMENT(#5081,1.);
#5074=DERIVED_UNIT_ELEMENT(#10294,-3.);
#5075=DERIVED_UNIT_ELEMENT(#5081,1.);
#5076=DERIVED_UNIT_ELEMENT(#10294,-3.);
#5077=DERIVED_UNIT_ELEMENT(#5081,1.);
#5078=DERIVED_UNIT_ELEMENT(#10294,-3.);
#5079=DERIVED_UNIT_ELEMENT(#5081,1.);
#5080=DERIVED_UNIT_ELEMENT(#10294,-3.);
#5081=(
MASS_UNIT()
NAMED_UNIT(*)
SI_UNIT(.KILO.,.GRAM.)
);
#5082=DERIVED_UNIT((#5035,#5036));
#5083=DERIVED_UNIT((#5037,#5038));
#5084=DERIVED_UNIT((#5039,#5040));
#5085=DERIVED_UNIT((#5041,#5042));
#5086=DERIVED_UNIT((#5043,#5044));
#5087=DERIVED_UNIT((#5045,#5046));
#5088=DERIVED_UNIT((#5047,#5048));
#5089=DERIVED_UNIT((#5049,#5050));
#5090=DERIVED_UNIT((#5051,#5052));
#5091=DERIVED_UNIT((#5053,#5054));
#5092=DERIVED_UNIT((#5055,#5056));
#5093=DERIVED_UNIT((#5057,#5058));
#5094=DERIVED_UNIT((#5059,#5060));
#5095=DERIVED_UNIT((#5061,#5062));
#5096=DERIVED_UNIT((#5063,#5064));
#5097=DERIVED_UNIT((#5065,#5066));
#5098=DERIVED_UNIT((#5067,#5068));
#5099=DERIVED_UNIT((#5069,#5070));
#5100=DERIVED_UNIT((#5071,#5072));
#5101=DERIVED_UNIT((#5073,#5074));
#5102=DERIVED_UNIT((#5075,#5076));
#5103=DERIVED_UNIT((#5077,#5078));
#5104=DERIVED_UNIT((#5079,#5080));
#5105=MEASURE_REPRESENTATION_ITEM('density measure',
POSITIVE_RATIO_MEASURE(7850.),#5082);
#5106=MEASURE_REPRESENTATION_ITEM('density measure',
POSITIVE_RATIO_MEASURE(7850.),#5083);
#5107=MEASURE_REPRESENTATION_ITEM('density measure',
POSITIVE_RATIO_MEASURE(7850.),#5084);
#5108=MEASURE_REPRESENTATION_ITEM('density measure',
POSITIVE_RATIO_MEASURE(7850.),#5085);
#5109=MEASURE_REPRESENTATION_ITEM('density measure',
POSITIVE_RATIO_MEASURE(7850.),#5086);
#5110=MEASURE_REPRESENTATION_ITEM('density measure',
POSITIVE_RATIO_MEASURE(7850.),#5087);
#5111=MEASURE_REPRESENTATION_ITEM('density measure',
POSITIVE_RATIO_MEASURE(7850.),#5088);
#5112=MEASURE_REPRESENTATION_ITEM('density measure',
POSITIVE_RATIO_MEASURE(7850.),#5089);
#5113=MEASURE_REPRESENTATION_ITEM('density measure',
POSITIVE_RATIO_MEASURE(7850.),#5090);
#5114=MEASURE_REPRESENTATION_ITEM('density measure',
POSITIVE_RATIO_MEASURE(7850.),#5091);
#5115=MEASURE_REPRESENTATION_ITEM('density measure',
POSITIVE_RATIO_MEASURE(7850.),#5092);
#5116=MEASURE_REPRESENTATION_ITEM('density measure',
POSITIVE_RATIO_MEASURE(7850.),#5093);
#5117=MEASURE_REPRESENTATION_ITEM('density measure',
POSITIVE_RATIO_MEASURE(7850.),#5094);
#5118=MEASURE_REPRESENTATION_ITEM('density measure',
POSITIVE_RATIO_MEASURE(7850.),#5095);
#5119=MEASURE_REPRESENTATION_ITEM('density measure',
POSITIVE_RATIO_MEASURE(7850.),#5096);
#5120=MEASURE_REPRESENTATION_ITEM('density measure',
POSITIVE_RATIO_MEASURE(7850.),#5097);
#5121=MEASURE_REPRESENTATION_ITEM('density measure',
POSITIVE_RATIO_MEASURE(7850.),#5098);
#5122=MEASURE_REPRESENTATION_ITEM('density measure',
POSITIVE_RATIO_MEASURE(7850.),#5099);
#5123=MEASURE_REPRESENTATION_ITEM('density measure',
POSITIVE_RATIO_MEASURE(7850.),#5100);
#5124=MEASURE_REPRESENTATION_ITEM('density measure',
POSITIVE_RATIO_MEASURE(7850.),#5101);
#5125=MEASURE_REPRESENTATION_ITEM('density measure',
POSITIVE_RATIO_MEASURE(7850.),#5102);
#5126=MEASURE_REPRESENTATION_ITEM('density measure',
POSITIVE_RATIO_MEASURE(7850.),#5103);
#5127=MEASURE_REPRESENTATION_ITEM('density measure',
POSITIVE_RATIO_MEASURE(7850.),#5104);
#5128=PROPERTY_DEFINITION_REPRESENTATION(#5243,#5174);
#5129=PROPERTY_DEFINITION_REPRESENTATION(#5244,#5175);
#5130=PROPERTY_DEFINITION_REPRESENTATION(#5245,#5176);
#5131=PROPERTY_DEFINITION_REPRESENTATION(#5246,#5177);
#5132=PROPERTY_DEFINITION_REPRESENTATION(#5247,#5178);
#5133=PROPERTY_DEFINITION_REPRESENTATION(#5248,#5179);
#5134=PROPERTY_DEFINITION_REPRESENTATION(#5249,#5180);
#5135=PROPERTY_DEFINITION_REPRESENTATION(#5250,#5181);
#5136=PROPERTY_DEFINITION_REPRESENTATION(#5251,#5182);
#5137=PROPERTY_DEFINITION_REPRESENTATION(#5252,#5183);
#5138=PROPERTY_DEFINITION_REPRESENTATION(#5253,#5184);
#5139=PROPERTY_DEFINITION_REPRESENTATION(#5254,#5185);
#5140=PROPERTY_DEFINITION_REPRESENTATION(#5255,#5186);
#5141=PROPERTY_DEFINITION_REPRESENTATION(#5256,#5187);
#5142=PROPERTY_DEFINITION_REPRESENTATION(#5257,#5188);
#5143=PROPERTY_DEFINITION_REPRESENTATION(#5258,#5189);
#5144=PROPERTY_DEFINITION_REPRESENTATION(#5259,#5190);
#5145=PROPERTY_DEFINITION_REPRESENTATION(#5260,#5191);
#5146=PROPERTY_DEFINITION_REPRESENTATION(#5261,#5192);
#5147=PROPERTY_DEFINITION_REPRESENTATION(#5262,#5193);
#5148=PROPERTY_DEFINITION_REPRESENTATION(#5263,#5194);
#5149=PROPERTY_DEFINITION_REPRESENTATION(#5264,#5195);
#5150=PROPERTY_DEFINITION_REPRESENTATION(#5265,#5196);
#5151=PROPERTY_DEFINITION_REPRESENTATION(#5266,#5197);
#5152=PROPERTY_DEFINITION_REPRESENTATION(#5267,#5198);
#5153=PROPERTY_DEFINITION_REPRESENTATION(#5268,#5199);
#5154=PROPERTY_DEFINITION_REPRESENTATION(#5269,#5200);
#5155=PROPERTY_DEFINITION_REPRESENTATION(#5270,#5201);
#5156=PROPERTY_DEFINITION_REPRESENTATION(#5271,#5202);
#5157=PROPERTY_DEFINITION_REPRESENTATION(#5272,#5203);
#5158=PROPERTY_DEFINITION_REPRESENTATION(#5273,#5204);
#5159=PROPERTY_DEFINITION_REPRESENTATION(#5274,#5205);
#5160=PROPERTY_DEFINITION_REPRESENTATION(#5275,#5206);
#5161=PROPERTY_DEFINITION_REPRESENTATION(#5276,#5207);
#5162=PROPERTY_DEFINITION_REPRESENTATION(#5277,#5208);
#5163=PROPERTY_DEFINITION_REPRESENTATION(#5278,#5209);
#5164=PROPERTY_DEFINITION_REPRESENTATION(#5279,#5210);
#5165=PROPERTY_DEFINITION_REPRESENTATION(#5280,#5211);
#5166=PROPERTY_DEFINITION_REPRESENTATION(#5281,#5212);
#5167=PROPERTY_DEFINITION_REPRESENTATION(#5282,#5213);
#5168=PROPERTY_DEFINITION_REPRESENTATION(#5283,#5214);
#5169=PROPERTY_DEFINITION_REPRESENTATION(#5284,#5215);
#5170=PROPERTY_DEFINITION_REPRESENTATION(#5285,#5216);
#5171=PROPERTY_DEFINITION_REPRESENTATION(#5286,#5217);
#5172=PROPERTY_DEFINITION_REPRESENTATION(#5287,#5218);
#5173=PROPERTY_DEFINITION_REPRESENTATION(#5288,#5219);
#5174=REPRESENTATION('material name',(#5220),#10267);
#5175=REPRESENTATION('density',(#5105),#10267);
#5176=REPRESENTATION('material name',(#5221),#10268);
#5177=REPRESENTATION('density',(#5106),#10268);
#5178=REPRESENTATION('material name',(#5222),#10269);
#5179=REPRESENTATION('density',(#5107),#10269);
#5180=REPRESENTATION('material name',(#5223),#10270);
#5181=REPRESENTATION('density',(#5108),#10270);
#5182=REPRESENTATION('material name',(#5224),#10271);
#5183=REPRESENTATION('density',(#5109),#10271);
#5184=REPRESENTATION('material name',(#5225),#10272);
#5185=REPRESENTATION('density',(#5110),#10272);
#5186=REPRESENTATION('material name',(#5226),#10273);
#5187=REPRESENTATION('density',(#5111),#10273);
#5188=REPRESENTATION('material name',(#5227),#10274);
#5189=REPRESENTATION('density',(#5112),#10274);
#5190=REPRESENTATION('material name',(#5228),#10275);
#5191=REPRESENTATION('density',(#5113),#10275);
#5192=REPRESENTATION('material name',(#5229),#10276);
#5193=REPRESENTATION('density',(#5114),#10276);
#5194=REPRESENTATION('material name',(#5230),#10277);
#5195=REPRESENTATION('density',(#5115),#10277);
#5196=REPRESENTATION('material name',(#5231),#10278);
#5197=REPRESENTATION('density',(#5116),#10278);
#5198=REPRESENTATION('material name',(#5232),#10279);
#5199=REPRESENTATION('density',(#5117),#10279);
#5200=REPRESENTATION('material name',(#5233),#10281);
#5201=REPRESENTATION('density',(#5118),#10281);
#5202=REPRESENTATION('material name',(#5234),#10282);
#5203=REPRESENTATION('density',(#5119),#10282);
#5204=REPRESENTATION('material name',(#5235),#10284);
#5205=REPRESENTATION('density',(#5120),#10284);
#5206=REPRESENTATION('material name',(#5236),#10285);
#5207=REPRESENTATION('density',(#5121),#10285);
#5208=REPRESENTATION('material name',(#5237),#10286);
#5209=REPRESENTATION('density',(#5122),#10286);
#5210=REPRESENTATION('material name',(#5238),#10287);
#5211=REPRESENTATION('density',(#5123),#10287);
#5212=REPRESENTATION('material name',(#5239),#10288);
#5213=REPRESENTATION('density',(#5124),#10288);
#5214=REPRESENTATION('material name',(#5240),#10289);
#5215=REPRESENTATION('density',(#5125),#10289);
#5216=REPRESENTATION('material name',(#5241),#10290);
#5217=REPRESENTATION('density',(#5126),#10290);
#5218=REPRESENTATION('material name',(#5242),#10291);
#5219=REPRESENTATION('density',(#5127),#10291);
#5220=DESCRIPTIVE_REPRESENTATION_ITEM('Steel','Steel');
#5221=DESCRIPTIVE_REPRESENTATION_ITEM('Steel','Steel');
#5222=DESCRIPTIVE_REPRESENTATION_ITEM('Steel','Steel');
#5223=DESCRIPTIVE_REPRESENTATION_ITEM('Steel','Steel');
#5224=DESCRIPTIVE_REPRESENTATION_ITEM('Steel','Steel');
#5225=DESCRIPTIVE_REPRESENTATION_ITEM('Steel','Steel');
#5226=DESCRIPTIVE_REPRESENTATION_ITEM('Steel','Steel');
#5227=DESCRIPTIVE_REPRESENTATION_ITEM('Steel','Steel');
#5228=DESCRIPTIVE_REPRESENTATION_ITEM('Steel','Steel');
#5229=DESCRIPTIVE_REPRESENTATION_ITEM('Steel','Steel');
#5230=DESCRIPTIVE_REPRESENTATION_ITEM('Steel','Steel');
#5231=DESCRIPTIVE_REPRESENTATION_ITEM('Steel','Steel');
#5232=DESCRIPTIVE_REPRESENTATION_ITEM('Steel','Steel');
#5233=DESCRIPTIVE_REPRESENTATION_ITEM('Steel','Steel');
#5234=DESCRIPTIVE_REPRESENTATION_ITEM('Steel','Steel');
#5235=DESCRIPTIVE_REPRESENTATION_ITEM('Steel','Steel');
#5236=DESCRIPTIVE_REPRESENTATION_ITEM('Steel','Steel');
#5237=DESCRIPTIVE_REPRESENTATION_ITEM('Steel','Steel');
#5238=DESCRIPTIVE_REPRESENTATION_ITEM('Steel','Steel');
#5239=DESCRIPTIVE_REPRESENTATION_ITEM('Steel','Steel');
#5240=DESCRIPTIVE_REPRESENTATION_ITEM('Steel','Steel');
#5241=DESCRIPTIVE_REPRESENTATION_ITEM('Steel','Steel');
#5242=DESCRIPTIVE_REPRESENTATION_ITEM('Steel','Steel');
#5243=PROPERTY_DEFINITION('material property','material name',#10443);
#5244=PROPERTY_DEFINITION('material property','density of part',#10443);
#5245=PROPERTY_DEFINITION('material property','material name',#10444);
#5246=PROPERTY_DEFINITION('material property','density of part',#10444);
#5247=PROPERTY_DEFINITION('material property','material name',#10445);
#5248=PROPERTY_DEFINITION('material property','density of part',#10445);
#5249=PROPERTY_DEFINITION('material property','material name',#10446);
#5250=PROPERTY_DEFINITION('material property','density of part',#10446);
#5251=PROPERTY_DEFINITION('material property','material name',#10447);
#5252=PROPERTY_DEFINITION('material property','density of part',#10447);
#5253=PROPERTY_DEFINITION('material property','material name',#10448);
#5254=PROPERTY_DEFINITION('material property','density of part',#10448);
#5255=PROPERTY_DEFINITION('material property','material name',#10449);
#5256=PROPERTY_DEFINITION('material property','density of part',#10449);
#5257=PROPERTY_DEFINITION('material property','material name',#10450);
#5258=PROPERTY_DEFINITION('material property','density of part',#10450);
#5259=PROPERTY_DEFINITION('material property','material name',#10451);
#5260=PROPERTY_DEFINITION('material property','density of part',#10451);
#5261=PROPERTY_DEFINITION('material property','material name',#10452);
#5262=PROPERTY_DEFINITION('material property','density of part',#10452);
#5263=PROPERTY_DEFINITION('material property','material name',#10453);
#5264=PROPERTY_DEFINITION('material property','density of part',#10453);
#5265=PROPERTY_DEFINITION('material property','material name',#10454);
#5266=PROPERTY_DEFINITION('material property','density of part',#10454);
#5267=PROPERTY_DEFINITION('material property','material name',#10455);
#5268=PROPERTY_DEFINITION('material property','density of part',#10455);
#5269=PROPERTY_DEFINITION('material property','material name',#10457);
#5270=PROPERTY_DEFINITION('material property','density of part',#10457);
#5271=PROPERTY_DEFINITION('material property','material name',#10458);
#5272=PROPERTY_DEFINITION('material property','density of part',#10458);
#5273=PROPERTY_DEFINITION('material property','material name',#10460);
#5274=PROPERTY_DEFINITION('material property','density of part',#10460);
#5275=PROPERTY_DEFINITION('material property','material name',#10461);
#5276=PROPERTY_DEFINITION('material property','density of part',#10461);
#5277=PROPERTY_DEFINITION('material property','material name',#10462);
#5278=PROPERTY_DEFINITION('material property','density of part',#10462);
#5279=PROPERTY_DEFINITION('material property','material name',#10463);
#5280=PROPERTY_DEFINITION('material property','density of part',#10463);
#5281=PROPERTY_DEFINITION('material property','material name',#10464);
#5282=PROPERTY_DEFINITION('material property','density of part',#10464);
#5283=PROPERTY_DEFINITION('material property','material name',#10465);
#5284=PROPERTY_DEFINITION('material property','density of part',#10465);
#5285=PROPERTY_DEFINITION('material property','material name',#10466);
#5286=PROPERTY_DEFINITION('material property','density of part',#10466);
#5287=PROPERTY_DEFINITION('material property','material name',#10467);
#5288=PROPERTY_DEFINITION('material property','density of part',#10467);
#5289=AXIS2_PLACEMENT_3D('',#7406,#5864,#5865);
#5290=AXIS2_PLACEMENT_3D('',#7407,#5866,#5867);
#5291=AXIS2_PLACEMENT_3D('',#7408,#5868,#5869);
#5292=AXIS2_PLACEMENT_3D('',#7409,#5870,#5871);
#5293=AXIS2_PLACEMENT_3D('',#7411,#5872,#5873);
#5294=AXIS2_PLACEMENT_3D('',#7414,#5875,#5876);
#5295=AXIS2_PLACEMENT_3D('',#7415,#5877,#5878);
#5296=AXIS2_PLACEMENT_3D('',#7417,#5879,#5880);
#5297=AXIS2_PLACEMENT_3D('',#7420,#5882,#5883);
#5298=AXIS2_PLACEMENT_3D('',#7421,#5884,#5885);
#5299=AXIS2_PLACEMENT_3D('',#7423,#5886,#5887);
#5300=AXIS2_PLACEMENT_3D('',#7426,#5889,#5890);
#5301=AXIS2_PLACEMENT_3D('',#7427,#5891,#5892);
#5302=AXIS2_PLACEMENT_3D('',#7429,#5893,#5894);
#5303=AXIS2_PLACEMENT_3D('',#7432,#5896,#5897);
#5304=AXIS2_PLACEMENT_3D('',#7433,#5898,#5899);
#5305=AXIS2_PLACEMENT_3D('',#7435,#5900,#5901);
#5306=AXIS2_PLACEMENT_3D('',#7438,#5903,#5904);
#5307=AXIS2_PLACEMENT_3D('',#7439,#5905,#5906);
#5308=AXIS2_PLACEMENT_3D('',#7441,#5907,#5908);
#5309=AXIS2_PLACEMENT_3D('',#7444,#5910,#5911);
#5310=AXIS2_PLACEMENT_3D('',#7445,#5912,#5913);
#5311=AXIS2_PLACEMENT_3D('',#7447,#5914,#5915);
#5312=AXIS2_PLACEMENT_3D('',#7450,#5917,#5918);
#5313=AXIS2_PLACEMENT_3D('',#7451,#5919,#5920);
#5314=AXIS2_PLACEMENT_3D('',#7453,#5921,#5922);
#5315=AXIS2_PLACEMENT_3D('',#7456,#5924,#5925);
#5316=AXIS2_PLACEMENT_3D('',#7457,#5926,#5927);
#5317=AXIS2_PLACEMENT_3D('',#7459,#5928,#5929);
#5318=AXIS2_PLACEMENT_3D('',#7462,#5931,#5932);
#5319=AXIS2_PLACEMENT_3D('',#7463,#5933,#5934);
#5320=AXIS2_PLACEMENT_3D('',#7465,#5935,#5936);
#5321=AXIS2_PLACEMENT_3D('',#7468,#5938,#5939);
#5322=AXIS2_PLACEMENT_3D('',#7469,#5940,#5941);
#5323=AXIS2_PLACEMENT_3D('',#7471,#5942,#5943);
#5324=AXIS2_PLACEMENT_3D('',#7474,#5945,#5946);
#5325=AXIS2_PLACEMENT_3D('',#7475,#5947,#5948);
#5326=AXIS2_PLACEMENT_3D('',#7477,#5949,#5950);
#5327=AXIS2_PLACEMENT_3D('',#7480,#5952,#5953);
#5328=AXIS2_PLACEMENT_3D('',#7481,#5954,#5955);
#5329=AXIS2_PLACEMENT_3D('',#7483,#5956,#5957);
#5330=AXIS2_PLACEMENT_3D('',#7486,#5959,#5960);
#5331=AXIS2_PLACEMENT_3D('',#7487,#5961,#5962);
#5332=AXIS2_PLACEMENT_3D('',#7489,#5963,#5964);
#5333=AXIS2_PLACEMENT_3D('',#7492,#5966,#5967);
#5334=AXIS2_PLACEMENT_3D('',#7493,#5968,#5969);
#5335=AXIS2_PLACEMENT_3D('',#7495,#5970,#5971);
#5336=AXIS2_PLACEMENT_3D('',#7498,#5973,#5974);
#5337=AXIS2_PLACEMENT_3D('',#7499,#5975,#5976);
#5338=AXIS2_PLACEMENT_3D('',#7501,#5977,#5978);
#5339=AXIS2_PLACEMENT_3D('',#7504,#5980,#5981);
#5340=AXIS2_PLACEMENT_3D('',#7505,#5982,#5983);
#5341=AXIS2_PLACEMENT_3D('',#7514,#5988,#5989);
#5342=AXIS2_PLACEMENT_3D('',#7520,#5993,#5994);
#5343=AXIS2_PLACEMENT_3D('',#7526,#5998,#5999);
#5344=AXIS2_PLACEMENT_3D('',#7529,#6002,#6003);
#5345=AXIS2_PLACEMENT_3D('',#7530,#6004,#6005);
#5346=AXIS2_PLACEMENT_3D('',#7531,#6006,#6007);
#5347=AXIS2_PLACEMENT_3D('',#7532,#6008,#6009);
#5348=AXIS2_PLACEMENT_3D('',#7534,#6010,#6011);
#5349=AXIS2_PLACEMENT_3D('',#7537,#6013,#6014);
#5350=AXIS2_PLACEMENT_3D('',#7538,#6015,#6016);
#5351=AXIS2_PLACEMENT_3D('',#7540,#6017,#6018);
#5352=AXIS2_PLACEMENT_3D('',#7542,#6020,#6021);
#5353=AXIS2_PLACEMENT_3D('',#7543,#6022,#6023);
#5354=AXIS2_PLACEMENT_3D('',#7545,#6024,#6025);
#5355=AXIS2_PLACEMENT_3D('',#7547,#6027,#6028);
#5356=AXIS2_PLACEMENT_3D('',#7548,#6029,#6030);
#5357=AXIS2_PLACEMENT_3D('',#7549,#6031,#6032);
#5358=AXIS2_PLACEMENT_3D('',#7553,#6034,#6035);
#5359=AXIS2_PLACEMENT_3D('',#7554,#6036,#6037);
#5360=AXIS2_PLACEMENT_3D('',#7558,#6039,#6040);
#5361=AXIS2_PLACEMENT_3D('',#7560,#6042,#6043);
#5362=AXIS2_PLACEMENT_3D('',#7565,#6045,#6046);
#5363=AXIS2_PLACEMENT_3D('',#7568,#6048,#6049);
#5364=AXIS2_PLACEMENT_3D('',#7569,#6050,#6051);
#5365=AXIS2_PLACEMENT_3D('',#7571,#6053,#6054);
#5366=AXIS2_PLACEMENT_3D('',#7582,#6060,#6061);
#5367=AXIS2_PLACEMENT_3D('',#7583,#6062,#6063);
#5368=AXIS2_PLACEMENT_3D('',#7590,#6067,#6068);
#5369=AXIS2_PLACEMENT_3D('',#7591,#6069,#6070);
#5370=AXIS2_PLACEMENT_3D('',#7602,#6076,#6077);
#5371=AXIS2_PLACEMENT_3D('',#7603,#6078,#6079);
#5372=AXIS2_PLACEMENT_3D('',#7605,#6080,#6081);
#5373=AXIS2_PLACEMENT_3D('',#7608,#6083,#6084);
#5374=AXIS2_PLACEMENT_3D('',#7609,#6085,#6086);
#5375=AXIS2_PLACEMENT_3D('',#7612,#6088,#6089);
#5376=AXIS2_PLACEMENT_3D('',#7613,#6090,#6091);
#5377=AXIS2_PLACEMENT_3D('',#7615,#6092,#6093);
#5378=AXIS2_PLACEMENT_3D('',#7617,#6095,#6096);
#5379=AXIS2_PLACEMENT_3D('',#7619,#6097,#6098);
#5380=AXIS2_PLACEMENT_3D('',#7621,#6100,#6101);
#5381=AXIS2_PLACEMENT_3D('',#7623,#6102,#6103);
#5382=AXIS2_PLACEMENT_3D('',#7626,#6105,#6106);
#5383=AXIS2_PLACEMENT_3D('',#7627,#6107,#6108);
#5384=AXIS2_PLACEMENT_3D('',#7644,#6118,#6119);
#5385=AXIS2_PLACEMENT_3D('',#7648,#6122,#6123);
#5386=AXIS2_PLACEMENT_3D('',#7652,#6126,#6127);
#5387=AXIS2_PLACEMENT_3D('',#7654,#6129,#6130);
#5388=AXIS2_PLACEMENT_3D('',#7658,#6133,#6134);
#5389=AXIS2_PLACEMENT_3D('',#7662,#6137,#6138);
#5390=AXIS2_PLACEMENT_3D('',#7666,#6141,#6142);
#5391=AXIS2_PLACEMENT_3D('',#7670,#6145,#6146);
#5392=AXIS2_PLACEMENT_3D('',#7674,#6149,#6150);
#5393=AXIS2_PLACEMENT_3D('',#7676,#6152,#6153);
#5394=AXIS2_PLACEMENT_3D('',#7677,#6154,#6155);
#5395=AXIS2_PLACEMENT_3D('',#7678,#6156,#6157);
#5396=AXIS2_PLACEMENT_3D('',#7687,#6162,#6163);
#5397=AXIS2_PLACEMENT_3D('',#7693,#6167,#6168);
#5398=AXIS2_PLACEMENT_3D('',#7699,#6172,#6173);
#5399=AXIS2_PLACEMENT_3D('',#7705,#6177,#6178);
#5400=AXIS2_PLACEMENT_3D('',#7711,#6182,#6183);
#5401=AXIS2_PLACEMENT_3D('',#7714,#6186,#6187);
#5402=AXIS2_PLACEMENT_3D('',#7715,#6188,#6189);
#5403=AXIS2_PLACEMENT_3D('',#7716,#6190,#6191);
#5404=AXIS2_PLACEMENT_3D('',#7718,#6192,#6193);
#5405=AXIS2_PLACEMENT_3D('',#7719,#6194,#6195);
#5406=AXIS2_PLACEMENT_3D('',#7721,#6196,#6197);
#5407=AXIS2_PLACEMENT_3D('',#7722,#6198,#6199);
#5408=AXIS2_PLACEMENT_3D('',#7724,#6200,#6201);
#5409=AXIS2_PLACEMENT_3D('',#7726,#6203,#6204);
#5410=AXIS2_PLACEMENT_3D('',#7728,#6205,#6206);
#5411=AXIS2_PLACEMENT_3D('',#7730,#6208,#6209);
#5412=AXIS2_PLACEMENT_3D('',#7732,#6210,#6211);
#5413=AXIS2_PLACEMENT_3D('',#7734,#6213,#6214);
#5414=AXIS2_PLACEMENT_3D('',#7736,#6215,#6216);
#5415=AXIS2_PLACEMENT_3D('',#7737,#6217,#6218);
#5416=AXIS2_PLACEMENT_3D('',#7739,#6219,#6220);
#5417=AXIS2_PLACEMENT_3D('',#7741,#6222,#6223);
#5418=AXIS2_PLACEMENT_3D('',#7743,#6225,#6226);
#5419=AXIS2_PLACEMENT_3D('',#7744,#6227,#6228);
#5420=AXIS2_PLACEMENT_3D('',#7746,#6229,#6230);
#5421=AXIS2_PLACEMENT_3D('',#7749,#6232,#6233);
#5422=AXIS2_PLACEMENT_3D('',#7750,#6234,#6235);
#5423=AXIS2_PLACEMENT_3D('',#7752,#6236,#6237);
#5424=AXIS2_PLACEMENT_3D('',#7753,#6238,#6239);
#5425=AXIS2_PLACEMENT_3D('',#7755,#6240,#6241);
#5426=AXIS2_PLACEMENT_3D('',#7758,#6243,#6244);
#5427=AXIS2_PLACEMENT_3D('',#7759,#6245,#6246);
#5428=AXIS2_PLACEMENT_3D('',#7761,#6247,#6248);
#5429=AXIS2_PLACEMENT_3D('',#7762,#6249,#6250);
#5430=AXIS2_PLACEMENT_3D('',#7764,#6251,#6252);
#5431=AXIS2_PLACEMENT_3D('',#7766,#6254,#6255);
#5432=AXIS2_PLACEMENT_3D('',#7768,#6256,#6257);
#5433=AXIS2_PLACEMENT_3D('',#7770,#6259,#6260);
#5434=AXIS2_PLACEMENT_3D('',#7779,#6265,#6266);
#5435=AXIS2_PLACEMENT_3D('',#7785,#6270,#6271);
#5436=AXIS2_PLACEMENT_3D('',#7791,#6275,#6276);
#5437=AXIS2_PLACEMENT_3D('',#7794,#6279,#6280);
#5438=AXIS2_PLACEMENT_3D('',#7795,#6281,#6282);
#5439=AXIS2_PLACEMENT_3D('',#7796,#6283,#6284);
#5440=AXIS2_PLACEMENT_3D('',#7797,#6285,#6286);
#5441=AXIS2_PLACEMENT_3D('',#7806,#6291,#6292);
#5442=AXIS2_PLACEMENT_3D('',#7812,#6296,#6297);
#5443=AXIS2_PLACEMENT_3D('',#7818,#6301,#6302);
#5444=AXIS2_PLACEMENT_3D('',#7821,#6305,#6306);
#5445=AXIS2_PLACEMENT_3D('',#7822,#6307,#6308);
#5446=AXIS2_PLACEMENT_3D('',#7823,#6309,#6310);
#5447=AXIS2_PLACEMENT_3D('',#7824,#6311,#6312);
#5448=AXIS2_PLACEMENT_3D('',#7826,#6313,#6314);
#5449=AXIS2_PLACEMENT_3D('',#7829,#6316,#6317);
#5450=AXIS2_PLACEMENT_3D('',#7830,#6318,#6319);
#5451=AXIS2_PLACEMENT_3D('',#7832,#6320,#6321);
#5452=AXIS2_PLACEMENT_3D('',#7835,#6323,#6324);
#5453=AXIS2_PLACEMENT_3D('',#7836,#6325,#6326);
#5454=AXIS2_PLACEMENT_3D('',#7838,#6327,#6328);
#5455=AXIS2_PLACEMENT_3D('',#7841,#6330,#6331);
#5456=AXIS2_PLACEMENT_3D('',#7842,#6332,#6333);
#5457=AXIS2_PLACEMENT_3D('',#7844,#6334,#6335);
#5458=AXIS2_PLACEMENT_3D('',#7847,#6337,#6338);
#5459=AXIS2_PLACEMENT_3D('',#7848,#6339,#6340);
#5460=AXIS2_PLACEMENT_3D('',#7850,#6341,#6342);
#5461=AXIS2_PLACEMENT_3D('',#7853,#6344,#6345);
#5462=AXIS2_PLACEMENT_3D('',#7854,#6346,#6347);
#5463=AXIS2_PLACEMENT_3D('',#7863,#6352,#6353);
#5464=AXIS2_PLACEMENT_3D('',#7869,#6357,#6358);
#5465=AXIS2_PLACEMENT_3D('',#7875,#6362,#6363);
#5466=AXIS2_PLACEMENT_3D('',#7877,#6365,#6366);
#5467=AXIS2_PLACEMENT_3D('',#7879,#6368,#6369);
#5468=AXIS2_PLACEMENT_3D('',#7888,#6374,#6375);
#5469=AXIS2_PLACEMENT_3D('',#7894,#6379,#6380);
#5470=AXIS2_PLACEMENT_3D('',#7900,#6384,#6385);
#5471=AXIS2_PLACEMENT_3D('',#7903,#6388,#6389);
#5472=AXIS2_PLACEMENT_3D('',#7904,#6390,#6391);
#5473=AXIS2_PLACEMENT_3D('',#7905,#6392,#6393);
#5474=AXIS2_PLACEMENT_3D('',#7906,#6394,#6395);
#5475=AXIS2_PLACEMENT_3D('',#7915,#6400,#6401);
#5476=AXIS2_PLACEMENT_3D('',#7921,#6405,#6406);
#5477=AXIS2_PLACEMENT_3D('',#7927,#6410,#6411);
#5478=AXIS2_PLACEMENT_3D('',#7933,#6415,#6416);
#5479=AXIS2_PLACEMENT_3D('',#7939,#6420,#6421);
#5480=AXIS2_PLACEMENT_3D('',#7942,#6424,#6425);
#5481=AXIS2_PLACEMENT_3D('',#7943,#6426,#6427);
#5482=AXIS2_PLACEMENT_3D('',#7944,#6428,#6429);
#5483=AXIS2_PLACEMENT_3D('',#7946,#6430,#6431);
#5484=AXIS2_PLACEMENT_3D('',#7947,#6432,#6433);
#5485=AXIS2_PLACEMENT_3D('',#7949,#6434,#6435);
#5486=AXIS2_PLACEMENT_3D('',#7950,#6436,#6437);
#5487=AXIS2_PLACEMENT_3D('',#7952,#6438,#6439);
#5488=AXIS2_PLACEMENT_3D('',#7954,#6441,#6442);
#5489=AXIS2_PLACEMENT_3D('',#7956,#6443,#6444);
#5490=AXIS2_PLACEMENT_3D('',#7958,#6446,#6447);
#5491=AXIS2_PLACEMENT_3D('',#7960,#6448,#6449);
#5492=AXIS2_PLACEMENT_3D('',#7962,#6451,#6452);
#5493=AXIS2_PLACEMENT_3D('',#7964,#6453,#6454);
#5494=AXIS2_PLACEMENT_3D('',#7965,#6455,#6456);
#5495=AXIS2_PLACEMENT_3D('',#7967,#6457,#6458);
#5496=AXIS2_PLACEMENT_3D('',#7969,#6460,#6461);
#5497=AXIS2_PLACEMENT_3D('',#7971,#6463,#6464);
#5498=AXIS2_PLACEMENT_3D('',#7972,#6465,#6466);
#5499=AXIS2_PLACEMENT_3D('',#7974,#6467,#6468);
#5500=AXIS2_PLACEMENT_3D('',#7977,#6470,#6471);
#5501=AXIS2_PLACEMENT_3D('',#7978,#6472,#6473);
#5502=AXIS2_PLACEMENT_3D('',#7980,#6474,#6475);
#5503=AXIS2_PLACEMENT_3D('',#7982,#6477,#6478);
#5504=AXIS2_PLACEMENT_3D('',#7983,#6479,#6480);
#5505=AXIS2_PLACEMENT_3D('',#7985,#6481,#6482);
#5506=AXIS2_PLACEMENT_3D('',#8011,#6484,#6485);
#5507=AXIS2_PLACEMENT_3D('',#8017,#6489,#6490);
#5508=AXIS2_PLACEMENT_3D('',#8021,#6493,#6494);
#5509=AXIS2_PLACEMENT_3D('',#8025,#6497,#6498);
#5510=AXIS2_PLACEMENT_3D('',#8029,#6501,#6502);
#5511=AXIS2_PLACEMENT_3D('',#8033,#6505,#6506);
#5512=AXIS2_PLACEMENT_3D('',#8035,#6508,#6509);
#5513=AXIS2_PLACEMENT_3D('',#8036,#6510,#6511);
#5514=AXIS2_PLACEMENT_3D('',#8037,#6512,#6513);
#5515=AXIS2_PLACEMENT_3D('',#8038,#6514,#6515);
#5516=AXIS2_PLACEMENT_3D('',#8050,#6517,#6518);
#5517=AXIS2_PLACEMENT_3D('',#8066,#6519,#6520);
#5518=AXIS2_PLACEMENT_3D('',#8068,#6521,#6522);
#5519=AXIS2_PLACEMENT_3D('',#8094,#6524,#6525);
#5520=AXIS2_PLACEMENT_3D('',#8097,#6528,#6529);
#5521=AXIS2_PLACEMENT_3D('',#8099,#6531,#6532);
#5522=AXIS2_PLACEMENT_3D('',#8101,#6534,#6535);
#5523=AXIS2_PLACEMENT_3D('',#8103,#6536,#6537);
#5524=AXIS2_PLACEMENT_3D('',#8106,#6539,#6540);
#5525=AXIS2_PLACEMENT_3D('',#8107,#6541,#6542);
#5526=AXIS2_PLACEMENT_3D('',#8109,#6544,#6545);
#5527=AXIS2_PLACEMENT_3D('',#8111,#6547,#6548);
#5528=AXIS2_PLACEMENT_3D('',#8112,#6549,#6550);
#5529=AXIS2_PLACEMENT_3D('',#8113,#6551,#6552);
#5530=AXIS2_PLACEMENT_3D('',#8114,#6553,#6554);
#5531=AXIS2_PLACEMENT_3D('',#9346,#6555,#6556);
#5532=AXIS2_PLACEMENT_3D('',#9471,#6557,#6558);
#5533=AXIS2_PLACEMENT_3D('',#9472,#6559,#6560);
#5534=AXIS2_PLACEMENT_3D('',#9473,#6561,#6562);
#5535=AXIS2_PLACEMENT_3D('',#9474,#6563,#6564);
#5536=AXIS2_PLACEMENT_3D('',#9475,#6565,#6566);
#5537=AXIS2_PLACEMENT_3D('',#9479,#6568,#6569);
#5538=AXIS2_PLACEMENT_3D('',#9480,#6570,#6571);
#5539=AXIS2_PLACEMENT_3D('',#9493,#6572,#6573);
#5540=AXIS2_PLACEMENT_3D('',#9534,#6575,#6576);
#5541=AXIS2_PLACEMENT_3D('',#9545,#6577,#6578);
#5542=AXIS2_PLACEMENT_3D('',#9547,#6580,#6581);
#5543=AXIS2_PLACEMENT_3D('',#9549,#6582,#6583);
#5544=AXIS2_PLACEMENT_3D('',#9552,#6585,#6586);
#5545=AXIS2_PLACEMENT_3D('',#9553,#6587,#6588);
#5546=AXIS2_PLACEMENT_3D('',#9555,#6589,#6590);
#5547=AXIS2_PLACEMENT_3D('',#9558,#6592,#6593);
#5548=AXIS2_PLACEMENT_3D('',#9559,#6594,#6595);
#5549=AXIS2_PLACEMENT_3D('',#9560,#6596,#6597);
#5550=AXIS2_PLACEMENT_3D('',#9561,#6598,#6599);
#5551=AXIS2_PLACEMENT_3D('',#9562,#6600,#6601);
#5552=AXIS2_PLACEMENT_3D('',#9571,#6606,#6607);
#5553=AXIS2_PLACEMENT_3D('',#9577,#6611,#6612);
#5554=AXIS2_PLACEMENT_3D('',#9583,#6616,#6617);
#5555=AXIS2_PLACEMENT_3D('',#9589,#6621,#6622);
#5556=AXIS2_PLACEMENT_3D('',#9595,#6626,#6627);
#5557=AXIS2_PLACEMENT_3D('',#9598,#6630,#6631);
#5558=AXIS2_PLACEMENT_3D('',#9599,#6632,#6633);
#5559=AXIS2_PLACEMENT_3D('',#9601,#6634,#6635);
#5560=AXIS2_PLACEMENT_3D('',#9602,#6636,#6637);
#5561=AXIS2_PLACEMENT_3D('',#9604,#6638,#6639);
#5562=AXIS2_PLACEMENT_3D('',#9606,#6641,#6642);
#5563=AXIS2_PLACEMENT_3D('',#9608,#6643,#6644);
#5564=AXIS2_PLACEMENT_3D('',#9610,#6646,#6647);
#5565=AXIS2_PLACEMENT_3D('',#9612,#6648,#6649);
#5566=AXIS2_PLACEMENT_3D('',#9614,#6651,#6652);
#5567=AXIS2_PLACEMENT_3D('',#9615,#6653,#6654);
#5568=AXIS2_PLACEMENT_3D('',#9616,#6655,#6656);
#5569=AXIS2_PLACEMENT_3D('',#9617,#6657,#6658);
#5570=AXIS2_PLACEMENT_3D('',#9619,#6659,#6660);
#5571=AXIS2_PLACEMENT_3D('',#9622,#6662,#6663);
#5572=AXIS2_PLACEMENT_3D('',#9623,#6664,#6665);
#5573=AXIS2_PLACEMENT_3D('',#9625,#6666,#6667);
#5574=AXIS2_PLACEMENT_3D('',#9628,#6669,#6670);
#5575=AXIS2_PLACEMENT_3D('',#9629,#6671,#6672);
#5576=AXIS2_PLACEMENT_3D('',#9631,#6673,#6674);
#5577=AXIS2_PLACEMENT_3D('',#9634,#6676,#6677);
#5578=AXIS2_PLACEMENT_3D('',#9635,#6678,#6679);
#5579=AXIS2_PLACEMENT_3D('',#9637,#6680,#6681);
#5580=AXIS2_PLACEMENT_3D('',#9640,#6683,#6684);
#5581=AXIS2_PLACEMENT_3D('',#9641,#6685,#6686);
#5582=AXIS2_PLACEMENT_3D('',#9643,#6687,#6688);
#5583=AXIS2_PLACEMENT_3D('',#9646,#6690,#6691);
#5584=AXIS2_PLACEMENT_3D('',#9647,#6692,#6693);
#5585=AXIS2_PLACEMENT_3D('',#9648,#6694,#6695);
#5586=AXIS2_PLACEMENT_3D('',#9650,#6696,#6697);
#5587=AXIS2_PLACEMENT_3D('',#9653,#6699,#6700);
#5588=AXIS2_PLACEMENT_3D('',#9654,#6701,#6702);
#5589=AXIS2_PLACEMENT_3D('',#9655,#6703,#6704);
#5590=AXIS2_PLACEMENT_3D('',#9657,#6705,#6706);
#5591=AXIS2_PLACEMENT_3D('',#9660,#6708,#6709);
#5592=AXIS2_PLACEMENT_3D('',#9661,#6710,#6711);
#5593=AXIS2_PLACEMENT_3D('',#9662,#6712,#6713);
#5594=AXIS2_PLACEMENT_3D('',#9664,#6714,#6715);
#5595=AXIS2_PLACEMENT_3D('',#9667,#6717,#6718);
#5596=AXIS2_PLACEMENT_3D('',#9668,#6719,#6720);
#5597=AXIS2_PLACEMENT_3D('',#9669,#6721,#6722);
#5598=AXIS2_PLACEMENT_3D('',#9671,#6723,#6724);
#5599=AXIS2_PLACEMENT_3D('',#9674,#6726,#6727);
#5600=AXIS2_PLACEMENT_3D('',#9675,#6728,#6729);
#5601=AXIS2_PLACEMENT_3D('',#9677,#6730,#6731);
#5602=AXIS2_PLACEMENT_3D('',#9680,#6733,#6734);
#5603=AXIS2_PLACEMENT_3D('',#9681,#6735,#6736);
#5604=AXIS2_PLACEMENT_3D('',#9690,#6741,#6742);
#5605=AXIS2_PLACEMENT_3D('',#9696,#6746,#6747);
#5606=AXIS2_PLACEMENT_3D('',#9702,#6751,#6752);
#5607=AXIS2_PLACEMENT_3D('',#9705,#6755,#6756);
#5608=AXIS2_PLACEMENT_3D('',#9706,#6757,#6758);
#5609=AXIS2_PLACEMENT_3D('',#9707,#6759,#6760);
#5610=AXIS2_PLACEMENT_3D('',#9708,#6761,#6762);
#5611=AXIS2_PLACEMENT_3D('',#9710,#6763,#6764);
#5612=AXIS2_PLACEMENT_3D('',#9713,#6766,#6767);
#5613=AXIS2_PLACEMENT_3D('',#9714,#6768,#6769);
#5614=AXIS2_PLACEMENT_3D('',#9716,#6770,#6771);
#5615=AXIS2_PLACEMENT_3D('',#9719,#6773,#6774);
#5616=AXIS2_PLACEMENT_3D('',#9720,#6775,#6776);
#5617=AXIS2_PLACEMENT_3D('',#9722,#6777,#6778);
#5618=AXIS2_PLACEMENT_3D('',#9725,#6780,#6781);
#5619=AXIS2_PLACEMENT_3D('',#9726,#6782,#6783);
#5620=AXIS2_PLACEMENT_3D('',#9728,#6784,#6785);
#5621=AXIS2_PLACEMENT_3D('',#9731,#6787,#6788);
#5622=AXIS2_PLACEMENT_3D('',#9732,#6789,#6790);
#5623=AXIS2_PLACEMENT_3D('',#9734,#6791,#6792);
#5624=AXIS2_PLACEMENT_3D('',#9737,#6794,#6795);
#5625=AXIS2_PLACEMENT_3D('',#9738,#6796,#6797);
#5626=AXIS2_PLACEMENT_3D('',#9747,#6802,#6803);
#5627=AXIS2_PLACEMENT_3D('',#9753,#6807,#6808);
#5628=AXIS2_PLACEMENT_3D('',#9759,#6812,#6813);
#5629=AXIS2_PLACEMENT_3D('',#9762,#6816,#6817);
#5630=AXIS2_PLACEMENT_3D('',#9763,#6818,#6819);
#5631=AXIS2_PLACEMENT_3D('',#9764,#6820,#6821);
#5632=AXIS2_PLACEMENT_3D('',#9765,#6822,#6823);
#5633=AXIS2_PLACEMENT_3D('',#9766,#6824,#6825);
#5634=AXIS2_PLACEMENT_3D('',#9769,#6826,#6827);
#5635=AXIS2_PLACEMENT_3D('',#9775,#6831,#6832);
#5636=AXIS2_PLACEMENT_3D('',#9781,#6836,#6837);
#5637=AXIS2_PLACEMENT_3D('',#9783,#6838,#6839);
#5638=AXIS2_PLACEMENT_3D('',#9787,#6842,#6843);
#5639=AXIS2_PLACEMENT_3D('',#9790,#6846,#6847);
#5640=AXIS2_PLACEMENT_3D('',#9791,#6848,#6849);
#5641=AXIS2_PLACEMENT_3D('',#9793,#6850,#6851);
#5642=AXIS2_PLACEMENT_3D('',#9795,#6852,#6853);
#5643=AXIS2_PLACEMENT_3D('',#9796,#6854,#6855);
#5644=AXIS2_PLACEMENT_3D('',#9798,#6856,#6857);
#5645=AXIS2_PLACEMENT_3D('',#9800,#6859,#6860);
#5646=AXIS2_PLACEMENT_3D('',#9802,#6861,#6862);
#5647=AXIS2_PLACEMENT_3D('',#9803,#6863,#6864);
#5648=AXIS2_PLACEMENT_3D('',#9805,#6865,#6866);
#5649=AXIS2_PLACEMENT_3D('',#9807,#6868,#6869);
#5650=AXIS2_PLACEMENT_3D('',#9809,#6870,#6871);
#5651=AXIS2_PLACEMENT_3D('',#9810,#6872,#6873);
#5652=AXIS2_PLACEMENT_3D('',#9812,#6874,#6875);
#5653=AXIS2_PLACEMENT_3D('',#9814,#6877,#6878);
#5654=AXIS2_PLACEMENT_3D('',#9816,#6879,#6880);
#5655=AXIS2_PLACEMENT_3D('',#9817,#6881,#6882);
#5656=AXIS2_PLACEMENT_3D('',#9819,#6883,#6884);
#5657=AXIS2_PLACEMENT_3D('',#9821,#6886,#6887);
#5658=AXIS2_PLACEMENT_3D('',#9823,#6888,#6889);
#5659=AXIS2_PLACEMENT_3D('',#9824,#6890,#6891);
#5660=AXIS2_PLACEMENT_3D('',#9826,#6892,#6893);
#5661=AXIS2_PLACEMENT_3D('',#9828,#6895,#6896);
#5662=AXIS2_PLACEMENT_3D('',#9830,#6897,#6898);
#5663=AXIS2_PLACEMENT_3D('',#9831,#6899,#6900);
#5664=AXIS2_PLACEMENT_3D('',#9833,#6902,#6903);
#5665=AXIS2_PLACEMENT_3D('',#9834,#6904,#6905);
#5666=AXIS2_PLACEMENT_3D('',#9837,#6906,#6907);
#5667=AXIS2_PLACEMENT_3D('',#9841,#6909,#6910);
#5668=AXIS2_PLACEMENT_3D('',#9843,#6912,#6913);
#5669=AXIS2_PLACEMENT_3D('',#9849,#6917,#6918);
#5670=AXIS2_PLACEMENT_3D('',#9851,#6919,#6920);
#5671=AXIS2_PLACEMENT_3D('',#9853,#6921,#6922);
#5672=AXIS2_PLACEMENT_3D('',#9855,#6924,#6925);
#5673=AXIS2_PLACEMENT_3D('',#9858,#6928,#6929);
#5674=AXIS2_PLACEMENT_3D('',#9860,#6930,#6931);
#5675=AXIS2_PLACEMENT_3D('',#9862,#6932,#6933);
#5676=AXIS2_PLACEMENT_3D('',#9863,#6934,#6935);
#5677=AXIS2_PLACEMENT_3D('',#9865,#6936,#6937);
#5678=AXIS2_PLACEMENT_3D('',#9867,#6939,#6940);
#5679=AXIS2_PLACEMENT_3D('',#9869,#6941,#6942);
#5680=AXIS2_PLACEMENT_3D('',#9870,#6943,#6944);
#5681=AXIS2_PLACEMENT_3D('',#9872,#6946,#6947);
#5682=AXIS2_PLACEMENT_3D('',#9873,#6948,#6949);
#5683=AXIS2_PLACEMENT_3D('',#9874,#6950,#6951);
#5684=AXIS2_PLACEMENT_3D('',#9875,#6952,#6953);
#5685=AXIS2_PLACEMENT_3D('',#9877,#6954,#6955);
#5686=AXIS2_PLACEMENT_3D('',#9880,#6957,#6958);
#5687=AXIS2_PLACEMENT_3D('',#9881,#6959,#6960);
#5688=AXIS2_PLACEMENT_3D('',#9883,#6961,#6962);
#5689=AXIS2_PLACEMENT_3D('',#9886,#6964,#6965);
#5690=AXIS2_PLACEMENT_3D('',#9887,#6966,#6967);
#5691=AXIS2_PLACEMENT_3D('',#9889,#6968,#6969);
#5692=AXIS2_PLACEMENT_3D('',#9892,#6971,#6972);
#5693=AXIS2_PLACEMENT_3D('',#9893,#6973,#6974);
#5694=AXIS2_PLACEMENT_3D('',#9895,#6975,#6976);
#5695=AXIS2_PLACEMENT_3D('',#9898,#6978,#6979);
#5696=AXIS2_PLACEMENT_3D('',#9899,#6980,#6981);
#5697=AXIS2_PLACEMENT_3D('',#9901,#6982,#6983);
#5698=AXIS2_PLACEMENT_3D('',#9904,#6985,#6986);
#5699=AXIS2_PLACEMENT_3D('',#9905,#6987,#6988);
#5700=AXIS2_PLACEMENT_3D('',#9907,#6989,#6990);
#5701=AXIS2_PLACEMENT_3D('',#9910,#6992,#6993);
#5702=AXIS2_PLACEMENT_3D('',#9911,#6994,#6995);
#5703=AXIS2_PLACEMENT_3D('',#9920,#7000,#7001);
#5704=AXIS2_PLACEMENT_3D('',#9926,#7005,#7006);
#5705=AXIS2_PLACEMENT_3D('',#9932,#7010,#7011);
#5706=AXIS2_PLACEMENT_3D('',#9935,#7014,#7015);
#5707=AXIS2_PLACEMENT_3D('',#9936,#7016,#7017);
#5708=AXIS2_PLACEMENT_3D('',#9937,#7018,#7019);
#5709=AXIS2_PLACEMENT_3D('',#9938,#7020,#7021);
#5710=AXIS2_PLACEMENT_3D('',#9940,#7022,#7023);
#5711=AXIS2_PLACEMENT_3D('',#9941,#7024,#7025);
#5712=AXIS2_PLACEMENT_3D('',#9943,#7026,#7027);
#5713=AXIS2_PLACEMENT_3D('',#9945,#7029,#7030);
#5714=AXIS2_PLACEMENT_3D('',#9947,#7031,#7032);
#5715=AXIS2_PLACEMENT_3D('',#9949,#7034,#7035);
#5716=AXIS2_PLACEMENT_3D('',#9951,#7036,#7037);
#5717=AXIS2_PLACEMENT_3D('',#9953,#7039,#7040);
#5718=AXIS2_PLACEMENT_3D('',#9955,#7041,#7042);
#5719=AXIS2_PLACEMENT_3D('',#9956,#7043,#7044);
#5720=AXIS2_PLACEMENT_3D('',#9958,#7045,#7046);
#5721=AXIS2_PLACEMENT_3D('',#9960,#7048,#7049);
#5722=AXIS2_PLACEMENT_3D('',#9962,#7050,#7051);
#5723=AXIS2_PLACEMENT_3D('',#9964,#7053,#7054);
#5724=AXIS2_PLACEMENT_3D('',#9966,#7055,#7056);
#5725=AXIS2_PLACEMENT_3D('',#9968,#7058,#7059);
#5726=AXIS2_PLACEMENT_3D('',#9969,#7060,#7061);
#5727=AXIS2_PLACEMENT_3D('',#9978,#7066,#7067);
#5728=AXIS2_PLACEMENT_3D('',#9984,#7071,#7072);
#5729=AXIS2_PLACEMENT_3D('',#9990,#7076,#7077);
#5730=AXIS2_PLACEMENT_3D('',#9996,#7081,#7082);
#5731=AXIS2_PLACEMENT_3D('',#10002,#7086,#7087);
#5732=AXIS2_PLACEMENT_3D('',#10005,#7090,#7091);
#5733=AXIS2_PLACEMENT_3D('',#10006,#7092,#7093);
#5734=AXIS2_PLACEMENT_3D('',#10007,#7094,#7095);
#5735=AXIS2_PLACEMENT_3D('',#10008,#7096,#7097);
#5736=AXIS2_PLACEMENT_3D('',#10010,#7098,#7099);
#5737=AXIS2_PLACEMENT_3D('',#10011,#7100,#7101);
#5738=AXIS2_PLACEMENT_3D('',#10013,#7102,#7103);
#5739=AXIS2_PLACEMENT_3D('',#10015,#7105,#7106);
#5740=AXIS2_PLACEMENT_3D('',#10017,#7107,#7108);
#5741=AXIS2_PLACEMENT_3D('',#10019,#7110,#7111);
#5742=AXIS2_PLACEMENT_3D('',#10021,#7112,#7113);
#5743=AXIS2_PLACEMENT_3D('',#10023,#7115,#7116);
#5744=AXIS2_PLACEMENT_3D('',#10025,#7117,#7118);
#5745=AXIS2_PLACEMENT_3D('',#10026,#7119,#7120);
#5746=AXIS2_PLACEMENT_3D('',#10028,#7121,#7122);
#5747=AXIS2_PLACEMENT_3D('',#10030,#7124,#7125);
#5748=AXIS2_PLACEMENT_3D('',#10032,#7126,#7127);
#5749=AXIS2_PLACEMENT_3D('',#10034,#7129,#7130);
#5750=AXIS2_PLACEMENT_3D('',#10036,#7131,#7132);
#5751=AXIS2_PLACEMENT_3D('',#10038,#7134,#7135);
#5752=AXIS2_PLACEMENT_3D('',#10039,#7136,#7137);
#5753=AXIS2_PLACEMENT_3D('',#10048,#7142,#7143);
#5754=AXIS2_PLACEMENT_3D('',#10054,#7147,#7148);
#5755=AXIS2_PLACEMENT_3D('',#10060,#7152,#7153);
#5756=AXIS2_PLACEMENT_3D('',#10066,#7157,#7158);
#5757=AXIS2_PLACEMENT_3D('',#10072,#7162,#7163);
#5758=AXIS2_PLACEMENT_3D('',#10075,#7166,#7167);
#5759=AXIS2_PLACEMENT_3D('',#10076,#7168,#7169);
#5760=AXIS2_PLACEMENT_3D('',#10077,#7170,#7171);
#5761=AXIS2_PLACEMENT_3D('',#10078,#7172,#7173);
#5762=AXIS2_PLACEMENT_3D('',#10079,#7174,#7175);
#5763=AXIS2_PLACEMENT_3D('',#10080,#7176,#7177);
#5764=AXIS2_PLACEMENT_3D('',#10081,#7178,#7179);
#5765=AXIS2_PLACEMENT_3D('',#10082,#7180,#7181);
#5766=AXIS2_PLACEMENT_3D('',#10083,#7182,#7183);
#5767=AXIS2_PLACEMENT_3D('',#10084,#7184,#7185);
#5768=AXIS2_PLACEMENT_3D('',#10085,#7186,#7187);
#5769=AXIS2_PLACEMENT_3D('',#10086,#7188,#7189);
#5770=AXIS2_PLACEMENT_3D('',#10087,#7190,#7191);
#5771=AXIS2_PLACEMENT_3D('',#10088,#7192,#7193);
#5772=AXIS2_PLACEMENT_3D('',#10089,#7194,#7195);
#5773=AXIS2_PLACEMENT_3D('',#10090,#7196,#7197);
#5774=AXIS2_PLACEMENT_3D('',#10091,#7198,#7199);
#5775=AXIS2_PLACEMENT_3D('',#10092,#7200,#7201);
#5776=AXIS2_PLACEMENT_3D('',#10093,#7202,#7203);
#5777=AXIS2_PLACEMENT_3D('',#10094,#7204,#7205);
#5778=AXIS2_PLACEMENT_3D('',#10095,#7206,#7207);
#5779=AXIS2_PLACEMENT_3D('',#10096,#7208,#7209);
#5780=AXIS2_PLACEMENT_3D('',#10097,#7210,#7211);
#5781=AXIS2_PLACEMENT_3D('',#10098,#7212,#7213);
#5782=AXIS2_PLACEMENT_3D('',#10099,#7214,#7215);
#5783=AXIS2_PLACEMENT_3D('',#10100,#7216,#7217);
#5784=AXIS2_PLACEMENT_3D('',#10101,#7218,#7219);
#5785=AXIS2_PLACEMENT_3D('',#10102,#7220,#7221);
#5786=AXIS2_PLACEMENT_3D('',#10103,#7222,#7223);
#5787=AXIS2_PLACEMENT_3D('',#10104,#7224,#7225);
#5788=AXIS2_PLACEMENT_3D('',#10105,#7226,#7227);
#5789=AXIS2_PLACEMENT_3D('',#10106,#7228,#7229);
#5790=AXIS2_PLACEMENT_3D('',#10107,#7230,#7231);
#5791=AXIS2_PLACEMENT_3D('',#10108,#7232,#7233);
#5792=AXIS2_PLACEMENT_3D('',#10109,#7234,#7235);
#5793=AXIS2_PLACEMENT_3D('',#10110,#7236,#7237);
#5794=AXIS2_PLACEMENT_3D('',#10111,#7238,#7239);
#5795=AXIS2_PLACEMENT_3D('',#10112,#7240,#7241);
#5796=AXIS2_PLACEMENT_3D('',#10113,#7242,#7243);
#5797=AXIS2_PLACEMENT_3D('',#10114,#7244,#7245);
#5798=AXIS2_PLACEMENT_3D('',#10115,#7246,#7247);
#5799=AXIS2_PLACEMENT_3D('',#10117,#7248,#7249);
#5800=AXIS2_PLACEMENT_3D('',#10120,#7251,#7252);
#5801=AXIS2_PLACEMENT_3D('',#10121,#7253,#7254);
#5802=AXIS2_PLACEMENT_3D('',#10123,#7255,#7256);
#5803=AXIS2_PLACEMENT_3D('',#10126,#7258,#7259);
#5804=AXIS2_PLACEMENT_3D('',#10127,#7260,#7261);
#5805=AXIS2_PLACEMENT_3D('',#10128,#7262,#7263);
#5806=AXIS2_PLACEMENT_3D('',#10129,#7264,#7265);
#5807=AXIS2_PLACEMENT_3D('',#10130,#7266,#7267);
#5808=AXIS2_PLACEMENT_3D('',#10132,#7268,#7269);
#5809=AXIS2_PLACEMENT_3D('',#10135,#7271,#7272);
#5810=AXIS2_PLACEMENT_3D('',#10136,#7273,#7274);
#5811=AXIS2_PLACEMENT_3D('',#10138,#7275,#7276);
#5812=AXIS2_PLACEMENT_3D('',#10141,#7278,#7279);
#5813=AXIS2_PLACEMENT_3D('',#10142,#7280,#7281);
#5814=AXIS2_PLACEMENT_3D('',#10143,#7282,#7283);
#5815=AXIS2_PLACEMENT_3D('',#10144,#7284,#7285);
#5816=AXIS2_PLACEMENT_3D('',#10145,#7286,#7287);
#5817=AXIS2_PLACEMENT_3D('',#10147,#7288,#7289);
#5818=AXIS2_PLACEMENT_3D('',#10148,#7290,#7291);
#5819=AXIS2_PLACEMENT_3D('',#10150,#7292,#7293);
#5820=AXIS2_PLACEMENT_3D('',#10152,#7295,#7296);
#5821=AXIS2_PLACEMENT_3D('',#10154,#7297,#7298);
#5822=AXIS2_PLACEMENT_3D('',#10156,#7300,#7301);
#5823=AXIS2_PLACEMENT_3D('',#10158,#7302,#7303);
#5824=AXIS2_PLACEMENT_3D('',#10160,#7305,#7306);
#5825=AXIS2_PLACEMENT_3D('',#10162,#7307,#7308);
#5826=AXIS2_PLACEMENT_3D('',#10163,#7309,#7310);
#5827=AXIS2_PLACEMENT_3D('',#10165,#7311,#7312);
#5828=AXIS2_PLACEMENT_3D('',#10167,#7314,#7315);
#5829=AXIS2_PLACEMENT_3D('',#10169,#7316,#7317);
#5830=AXIS2_PLACEMENT_3D('',#10171,#7319,#7320);
#5831=AXIS2_PLACEMENT_3D('',#10173,#7321,#7322);
#5832=AXIS2_PLACEMENT_3D('',#10175,#7324,#7325);
#5833=AXIS2_PLACEMENT_3D('',#10176,#7326,#7327);
#5834=AXIS2_PLACEMENT_3D('',#10185,#7332,#7333);
#5835=AXIS2_PLACEMENT_3D('',#10191,#7337,#7338);
#5836=AXIS2_PLACEMENT_3D('',#10197,#7342,#7343);
#5837=AXIS2_PLACEMENT_3D('',#10203,#7347,#7348);
#5838=AXIS2_PLACEMENT_3D('',#10209,#7352,#7353);
#5839=AXIS2_PLACEMENT_3D('',#10212,#7356,#7357);
#5840=AXIS2_PLACEMENT_3D('',#10213,#7358,#7359);
#5841=AXIS2_PLACEMENT_3D('',#10214,#7360,#7361);
#5842=AXIS2_PLACEMENT_3D('',#10215,#7362,#7363);
#5843=AXIS2_PLACEMENT_3D('',#10216,#7364,#7365);
#5844=AXIS2_PLACEMENT_3D('',#10217,#7366,#7367);
#5845=AXIS2_PLACEMENT_3D('',#10218,#7368,#7369);
#5846=AXIS2_PLACEMENT_3D('',#10219,#7370,#7371);
#5847=AXIS2_PLACEMENT_3D('',#10220,#7372,#7373);
#5848=AXIS2_PLACEMENT_3D('',#10221,#7374,#7375);
#5849=AXIS2_PLACEMENT_3D('',#10222,#7376,#7377);
#5850=AXIS2_PLACEMENT_3D('',#10223,#7378,#7379);
#5851=AXIS2_PLACEMENT_3D('',#10224,#7380,#7381);
#5852=AXIS2_PLACEMENT_3D('',#10225,#7382,#7383);
#5853=AXIS2_PLACEMENT_3D('',#10226,#7384,#7385);
#5854=AXIS2_PLACEMENT_3D('',#10227,#7386,#7387);
#5855=AXIS2_PLACEMENT_3D('',#10228,#7388,#7389);
#5856=AXIS2_PLACEMENT_3D('',#10229,#7390,#7391);
#5857=AXIS2_PLACEMENT_3D('',#10230,#7392,#7393);
#5858=AXIS2_PLACEMENT_3D('',#10231,#7394,#7395);
#5859=AXIS2_PLACEMENT_3D('',#10232,#7396,#7397);
#5860=AXIS2_PLACEMENT_3D('',#10233,#7398,#7399);
#5861=AXIS2_PLACEMENT_3D('',#10234,#7400,#7401);
#5862=AXIS2_PLACEMENT_3D('',#10235,#7402,#7403);
#5863=AXIS2_PLACEMENT_3D('',#10236,#7404,#7405);
#5864=DIRECTION('axis',(0.,0.,1.));
#5865=DIRECTION('refdir',(1.,0.,0.));
#5866=DIRECTION('axis',(0.,0.,1.));
#5867=DIRECTION('refdir',(1.,0.,0.));
#5868=DIRECTION('axis',(0.,0.,1.));
#5869=DIRECTION('refdir',(1.,0.,0.));
#5870=DIRECTION('center_axis',(0.,0.,1.));
#5871=DIRECTION('ref_axis',(1.,0.,0.));
#5872=DIRECTION('center_axis',(0.,0.,1.));
#5873=DIRECTION('ref_axis',(1.,0.,0.));
#5874=DIRECTION('',(0.,0.,1.));
#5875=DIRECTION('center_axis',(0.,0.,-1.));
#5876=DIRECTION('ref_axis',(1.,0.,0.));
#5877=DIRECTION('center_axis',(0.,0.,1.));
#5878=DIRECTION('ref_axis',(1.,0.,0.));
#5879=DIRECTION('center_axis',(0.,0.,1.));
#5880=DIRECTION('ref_axis',(1.,0.,0.));
#5881=DIRECTION('',(0.,0.,1.));
#5882=DIRECTION('center_axis',(0.,0.,-1.));
#5883=DIRECTION('ref_axis',(1.,0.,0.));
#5884=DIRECTION('center_axis',(0.,0.,1.));
#5885=DIRECTION('ref_axis',(1.,0.,0.));
#5886=DIRECTION('center_axis',(0.,0.,1.));
#5887=DIRECTION('ref_axis',(1.,0.,0.));
#5888=DIRECTION('',(0.,0.,1.));
#5889=DIRECTION('center_axis',(0.,0.,-1.));
#5890=DIRECTION('ref_axis',(1.,0.,0.));
#5891=DIRECTION('center_axis',(0.,0.,1.));
#5892=DIRECTION('ref_axis',(1.,0.,0.));
#5893=DIRECTION('center_axis',(0.,0.,1.));
#5894=DIRECTION('ref_axis',(1.,0.,0.));
#5895=DIRECTION('',(0.,0.,1.));
#5896=DIRECTION('center_axis',(0.,0.,-1.));
#5897=DIRECTION('ref_axis',(1.,0.,0.));
#5898=DIRECTION('center_axis',(0.,0.,1.));
#5899=DIRECTION('ref_axis',(1.,0.,0.));
#5900=DIRECTION('center_axis',(0.,0.,1.));
#5901=DIRECTION('ref_axis',(1.,0.,0.));
#5902=DIRECTION('',(0.,0.,1.));
#5903=DIRECTION('center_axis',(0.,0.,-1.));
#5904=DIRECTION('ref_axis',(1.,0.,0.));
#5905=DIRECTION('center_axis',(0.,0.,1.));
#5906=DIRECTION('ref_axis',(1.,0.,0.));
#5907=DIRECTION('center_axis',(0.,0.,1.));
#5908=DIRECTION('ref_axis',(1.,0.,0.));
#5909=DIRECTION('',(0.,0.,1.));
#5910=DIRECTION('center_axis',(0.,0.,-1.));
#5911=DIRECTION('ref_axis',(1.,0.,0.));
#5912=DIRECTION('center_axis',(0.,0.,1.));
#5913=DIRECTION('ref_axis',(1.,0.,0.));
#5914=DIRECTION('center_axis',(0.,0.,1.));
#5915=DIRECTION('ref_axis',(1.,0.,0.));
#5916=DIRECTION('',(0.,0.,1.));
#5917=DIRECTION('center_axis',(0.,0.,-1.));
#5918=DIRECTION('ref_axis',(1.,0.,0.));
#5919=DIRECTION('center_axis',(0.,0.,1.));
#5920=DIRECTION('ref_axis',(1.,0.,0.));
#5921=DIRECTION('center_axis',(0.,0.,1.));
#5922=DIRECTION('ref_axis',(1.,0.,0.));
#5923=DIRECTION('',(0.,0.,1.));
#5924=DIRECTION('center_axis',(0.,0.,-1.));
#5925=DIRECTION('ref_axis',(1.,0.,0.));
#5926=DIRECTION('center_axis',(0.,0.,1.));
#5927=DIRECTION('ref_axis',(1.,0.,0.));
#5928=DIRECTION('center_axis',(0.,0.,1.));
#5929=DIRECTION('ref_axis',(1.,0.,0.));
#5930=DIRECTION('',(0.,0.,1.));
#5931=DIRECTION('center_axis',(0.,0.,-1.));
#5932=DIRECTION('ref_axis',(1.,0.,0.));
#5933=DIRECTION('center_axis',(0.,0.,1.));
#5934=DIRECTION('ref_axis',(1.,0.,0.));
#5935=DIRECTION('center_axis',(0.,0.,1.));
#5936=DIRECTION('ref_axis',(1.,0.,0.));
#5937=DIRECTION('',(0.,0.,1.));
#5938=DIRECTION('center_axis',(0.,0.,-1.));
#5939=DIRECTION('ref_axis',(1.,0.,0.));
#5940=DIRECTION('center_axis',(0.,0.,1.));
#5941=DIRECTION('ref_axis',(1.,0.,0.));
#5942=DIRECTION('center_axis',(0.,0.,1.));
#5943=DIRECTION('ref_axis',(1.,0.,0.));
#5944=DIRECTION('',(0.,0.,1.));
#5945=DIRECTION('center_axis',(0.,0.,-1.));
#5946=DIRECTION('ref_axis',(1.,0.,0.));
#5947=DIRECTION('center_axis',(0.,0.,1.));
#5948=DIRECTION('ref_axis',(1.,0.,0.));
#5949=DIRECTION('center_axis',(0.,0.,1.));
#5950=DIRECTION('ref_axis',(1.,0.,0.));
#5951=DIRECTION('',(0.,0.,1.));
#5952=DIRECTION('center_axis',(0.,0.,-1.));
#5953=DIRECTION('ref_axis',(1.,0.,0.));
#5954=DIRECTION('center_axis',(0.,0.,1.));
#5955=DIRECTION('ref_axis',(1.,0.,0.));
#5956=DIRECTION('center_axis',(0.,0.,1.));
#5957=DIRECTION('ref_axis',(1.,0.,0.));
#5958=DIRECTION('',(0.,0.,1.));
#5959=DIRECTION('center_axis',(0.,0.,-1.));
#5960=DIRECTION('ref_axis',(1.,0.,0.));
#5961=DIRECTION('center_axis',(0.,0.,1.));
#5962=DIRECTION('ref_axis',(1.,0.,0.));
#5963=DIRECTION('center_axis',(0.,0.,1.));
#5964=DIRECTION('ref_axis',(1.,0.,0.));
#5965=DIRECTION('',(0.,0.,1.));
#5966=DIRECTION('center_axis',(0.,0.,-1.));
#5967=DIRECTION('ref_axis',(1.,0.,0.));
#5968=DIRECTION('center_axis',(0.,0.,1.));
#5969=DIRECTION('ref_axis',(1.,0.,0.));
#5970=DIRECTION('center_axis',(0.,0.,1.));
#5971=DIRECTION('ref_axis',(1.,0.,0.));
#5972=DIRECTION('',(0.,0.,1.));
#5973=DIRECTION('center_axis',(0.,0.,-1.));
#5974=DIRECTION('ref_axis',(1.,0.,0.));
#5975=DIRECTION('center_axis',(0.,0.,1.));
#5976=DIRECTION('ref_axis',(1.,0.,0.));
#5977=DIRECTION('center_axis',(0.,0.,1.));
#5978=DIRECTION('ref_axis',(1.,0.,0.));
#5979=DIRECTION('',(0.,0.,1.));
#5980=DIRECTION('center_axis',(0.,0.,-1.));
#5981=DIRECTION('ref_axis',(1.,0.,0.));
#5982=DIRECTION('center_axis',(0.,1.,0.));
#5983=DIRECTION('ref_axis',(-1.,0.,0.));
#5984=DIRECTION('',(-1.,0.,0.));
#5985=DIRECTION('',(0.,0.,1.));
#5986=DIRECTION('',(-1.,0.,0.));
#5987=DIRECTION('',(0.,0.,1.));
#5988=DIRECTION('center_axis',(1.,0.,0.));
#5989=DIRECTION('ref_axis',(0.,1.,0.));
#5990=DIRECTION('',(0.,1.,0.));
#5991=DIRECTION('',(0.,1.,0.));
#5992=DIRECTION('',(0.,0.,1.));
#5993=DIRECTION('center_axis',(0.,-1.,0.));
#5994=DIRECTION('ref_axis',(1.,0.,0.));
#5995=DIRECTION('',(1.,0.,0.));
#5996=DIRECTION('',(1.,0.,0.));
#5997=DIRECTION('',(0.,0.,1.));
#5998=DIRECTION('center_axis',(-1.,0.,0.));
#5999=DIRECTION('ref_axis',(0.,-1.,0.));
#6000=DIRECTION('',(0.,-1.,0.));
#6001=DIRECTION('',(0.,-1.,0.));
#6002=DIRECTION('center_axis',(0.,0.,1.));
#6003=DIRECTION('ref_axis',(1.,0.,0.));
#6004=DIRECTION('center_axis',(0.,0.,1.));
#6005=DIRECTION('ref_axis',(1.,0.,0.));
#6006=DIRECTION('axis',(0.,0.,1.));
#6007=DIRECTION('refdir',(1.,0.,0.));
#6008=DIRECTION('center_axis',(1.,0.,0.));
#6009=DIRECTION('ref_axis',(0.,0.,-1.));
#6010=DIRECTION('center_axis',(-1.,0.,0.));
#6011=DIRECTION('ref_axis',(0.,0.,-1.));
#6012=DIRECTION('',(-0.707106781186548,8.65956056235493E-17,-0.707106781186547));
#6013=DIRECTION('center_axis',(1.,0.,0.));
#6014=DIRECTION('ref_axis',(0.,0.,-1.));
#6015=DIRECTION('center_axis',(1.,0.,0.));
#6016=DIRECTION('ref_axis',(0.,0.,-1.));
#6017=DIRECTION('center_axis',(1.,0.,0.));
#6018=DIRECTION('ref_axis',(0.,0.,-1.));
#6019=DIRECTION('',(-1.,0.,0.));
#6020=DIRECTION('center_axis',(1.,0.,0.));
#6021=DIRECTION('ref_axis',(0.,0.,-1.));
#6022=DIRECTION('center_axis',(-1.,0.,0.));
#6023=DIRECTION('ref_axis',(0.,0.,-1.));
#6024=DIRECTION('center_axis',(-1.,0.,0.));
#6025=DIRECTION('ref_axis',(0.,0.,-1.));
#6026=DIRECTION('',(-0.707106781186553,-8.65956056235487E-17,0.707106781186542));
#6027=DIRECTION('center_axis',(1.,0.,0.));
#6028=DIRECTION('ref_axis',(0.,0.,-1.));
#6029=DIRECTION('axis',(0.,0.,1.));
#6030=DIRECTION('refdir',(1.,0.,0.));
#6031=DIRECTION('center_axis',(0.,0.,1.));
#6032=DIRECTION('ref_axis',(1.,0.,0.));
#6033=DIRECTION('',(0.,-1.,0.));
#6034=DIRECTION('center_axis',(0.,0.,1.));
#6035=DIRECTION('ref_axis',(1.,0.,0.));
#6036=DIRECTION('center_axis',(0.,0.,1.));
#6037=DIRECTION('ref_axis',(1.,0.,0.));
#6038=DIRECTION('',(0.,0.,1.));
#6039=DIRECTION('center_axis',(0.,0.,1.));
#6040=DIRECTION('ref_axis',(1.,0.,0.));
#6041=DIRECTION('',(0.,0.,-1.));
#6042=DIRECTION('center_axis',(0.,0.,1.));
#6043=DIRECTION('ref_axis',(-1.,1.22464679914735E-16,0.));
#6044=DIRECTION('',(0.,0.,-1.));
#6045=DIRECTION('center_axis',(0.,0.,1.));
#6046=DIRECTION('ref_axis',(1.,0.,0.));
#6047=DIRECTION('',(0.,0.,1.));
#6048=DIRECTION('center_axis',(0.,0.,1.));
#6049=DIRECTION('ref_axis',(1.,0.,0.));
#6050=DIRECTION('center_axis',(0.,0.,1.));
#6051=DIRECTION('ref_axis',(1.,0.,0.));
#6052=DIRECTION('',(0.,1.,0.));
#6053=DIRECTION('center_axis',(0.,0.,1.));
#6054=DIRECTION('ref_axis',(1.,0.,0.));
#6055=DIRECTION('',(0.,1.,0.));
#6056=DIRECTION('',(1.,0.,0.));
#6057=DIRECTION('',(0.,-1.,0.));
#6058=DIRECTION('',(-1.,0.,0.));
#6059=DIRECTION('',(0.,1.,0.));
#6060=DIRECTION('center_axis',(0.,0.,-1.));
#6061=DIRECTION('ref_axis',(1.,0.,0.));
#6062=DIRECTION('center_axis',(-1.,0.,0.));
#6063=DIRECTION('ref_axis',(0.,0.,1.));
#6064=DIRECTION('',(0.,0.,-1.));
#6065=DIRECTION('',(0.,1.,0.));
#6066=DIRECTION('',(0.,0.,1.));
#6067=DIRECTION('center_axis',(1.,0.,0.));
#6068=DIRECTION('ref_axis',(0.,0.,-1.));
#6069=DIRECTION('center_axis',(0.,0.,1.));
#6070=DIRECTION('ref_axis',(1.,0.,0.));
#6071=DIRECTION('',(0.,1.,0.));
#6072=DIRECTION('',(1.,0.,0.));
#6073=DIRECTION('',(0.,1.,0.));
#6074=DIRECTION('',(0.,1.,0.));
#6075=DIRECTION('',(-1.,0.,0.));
#6076=DIRECTION('center_axis',(0.,0.,-1.));
#6077=DIRECTION('ref_axis',(1.,0.,0.));
#6078=DIRECTION('center_axis',(1.,0.,0.));
#6079=DIRECTION('ref_axis',(0.,0.,-1.));
#6080=DIRECTION('center_axis',(1.,0.,0.));
#6081=DIRECTION('ref_axis',(0.,0.,-1.));
#6082=DIRECTION('',(1.,0.,0.));
#6083=DIRECTION('center_axis',(-1.,0.,0.));
#6084=DIRECTION('ref_axis',(0.,0.,-1.));
#6085=DIRECTION('center_axis',(1.,0.,0.));
#6086=DIRECTION('ref_axis',(0.,0.,-1.));
#6087=DIRECTION('',(1.,0.,0.));
#6088=DIRECTION('center_axis',(-1.,0.,0.));
#6089=DIRECTION('ref_axis',(0.,0.,-1.));
#6090=DIRECTION('center_axis',(0.,0.,1.));
#6091=DIRECTION('ref_axis',(1.,0.,0.));
#6092=DIRECTION('center_axis',(0.,0.,1.));
#6093=DIRECTION('ref_axis',(1.,0.,0.));
#6094=DIRECTION('',(0.,0.,1.));
#6095=DIRECTION('center_axis',(0.,0.,1.));
#6096=DIRECTION('ref_axis',(1.,0.,0.));
#6097=DIRECTION('center_axis',(0.,0.,1.));
#6098=DIRECTION('ref_axis',(1.,0.,0.));
#6099=DIRECTION('',(0.,0.,1.));
#6100=DIRECTION('center_axis',(0.,1.,0.));
#6101=DIRECTION('ref_axis',(1.,0.,0.));
#6102=DIRECTION('center_axis',(0.,1.,0.));
#6103=DIRECTION('ref_axis',(1.,0.,0.));
#6104=DIRECTION('',(0.,1.,0.));
#6105=DIRECTION('center_axis',(0.,-1.,0.));
#6106=DIRECTION('ref_axis',(1.,0.,0.));
#6107=DIRECTION('center_axis',(0.,-1.,0.));
#6108=DIRECTION('ref_axis',(0.,0.,-1.));
#6109=DIRECTION('',(0.,0.,-1.));
#6110=DIRECTION('',(1.,0.,0.));
#6111=DIRECTION('',(0.,0.,1.));
#6112=DIRECTION('',(0.,0.,1.));
#6113=DIRECTION('',(-1.,0.,0.));
#6114=DIRECTION('',(0.,0.,-1.));
#6115=DIRECTION('',(-1.,0.,0.));
#6116=DIRECTION('',(0.,0.,1.));
#6117=DIRECTION('',(-1.,0.,0.));
#6118=DIRECTION('center_axis',(-1.,0.,0.));
#6119=DIRECTION('ref_axis',(0.,0.,1.));
#6120=DIRECTION('',(0.,0.,1.));
#6121=DIRECTION('',(0.,1.,0.));
#6122=DIRECTION('center_axis',(0.,0.,-1.));
#6123=DIRECTION('ref_axis',(-1.,0.,0.));
#6124=DIRECTION('',(-1.,0.,0.));
#6125=DIRECTION('',(0.,1.,0.));
#6126=DIRECTION('center_axis',(1.,0.,0.));
#6127=DIRECTION('ref_axis',(0.,0.,-1.));
#6128=DIRECTION('',(0.,0.,-1.));
#6129=DIRECTION('center_axis',(1.,0.,0.));
#6130=DIRECTION('ref_axis',(0.,0.,-1.));
#6131=DIRECTION('',(0.,0.,-1.));
#6132=DIRECTION('',(0.,1.,0.));
#6133=DIRECTION('center_axis',(0.,0.,1.));
#6134=DIRECTION('ref_axis',(1.,0.,0.));
#6135=DIRECTION('',(1.,0.,0.));
#6136=DIRECTION('',(0.,1.,0.));
#6137=DIRECTION('center_axis',(-1.,0.,0.));
#6138=DIRECTION('ref_axis',(0.,0.,1.));
#6139=DIRECTION('',(0.,0.,1.));
#6140=DIRECTION('',(0.,1.,0.));
#6141=DIRECTION('center_axis',(0.,0.,1.));
#6142=DIRECTION('ref_axis',(1.,0.,0.));
#6143=DIRECTION('',(1.,0.,0.));
#6144=DIRECTION('',(0.,1.,0.));
#6145=DIRECTION('center_axis',(1.,0.,0.));
#6146=DIRECTION('ref_axis',(0.,0.,-1.));
#6147=DIRECTION('',(0.,0.,-1.));
#6148=DIRECTION('',(0.,1.,0.));
#6149=DIRECTION('center_axis',(0.,0.,1.));
#6150=DIRECTION('ref_axis',(1.,0.,0.));
#6151=DIRECTION('',(1.,0.,0.));
#6152=DIRECTION('center_axis',(0.,1.,0.));
#6153=DIRECTION('ref_axis',(0.,0.,1.));
#6154=DIRECTION('axis',(0.,0.,1.));
#6155=DIRECTION('refdir',(1.,0.,0.));
#6156=DIRECTION('center_axis',(0.866025403784439,0.,-0.5));
#6157=DIRECTION('ref_axis',(0.5,0.,0.866025403784439));
#6158=DIRECTION('',(-0.5,0.,-0.866025403784439));
#6159=DIRECTION('',(0.,-1.,0.));
#6160=DIRECTION('',(0.5,0.,0.866025403784439));
#6161=DIRECTION('',(0.,-1.,0.));
#6162=DIRECTION('center_axis',(1.20185167898973E-16,0.,-1.));
#6163=DIRECTION('ref_axis',(1.,0.,1.20185167898973E-16));
#6164=DIRECTION('',(-1.,0.,-1.20185167898973E-16));
#6165=DIRECTION('',(0.,-1.,0.));
#6166=DIRECTION('',(1.,0.,1.20185167898973E-16));
#6167=DIRECTION('center_axis',(-0.866025403784439,0.,-0.5));
#6168=DIRECTION('ref_axis',(0.5,0.,-0.866025403784439));
#6169=DIRECTION('',(-0.5,0.,0.866025403784439));
#6170=DIRECTION('',(0.,-1.,0.));
#6171=DIRECTION('',(0.5,0.,-0.866025403784439));
#6172=DIRECTION('center_axis',(-0.866025403784439,0.,0.5));
#6173=DIRECTION('ref_axis',(-0.5,0.,-0.866025403784439));
#6174=DIRECTION('',(0.5,0.,0.866025403784439));
#6175=DIRECTION('',(0.,-1.,0.));
#6176=DIRECTION('',(-0.5,0.,-0.866025403784439));
#6177=DIRECTION('center_axis',(-2.40370335797945E-16,0.,1.));
#6178=DIRECTION('ref_axis',(-1.,0.,-2.40370335797945E-16));
#6179=DIRECTION('',(1.,0.,2.40370335797945E-16));
#6180=DIRECTION('',(0.,-1.,0.));
#6181=DIRECTION('',(-1.,0.,-2.40370335797945E-16));
#6182=DIRECTION('center_axis',(0.866025403784439,0.,0.5));
#6183=DIRECTION('ref_axis',(-0.5,0.,0.866025403784439));
#6184=DIRECTION('',(0.5,0.,-0.866025403784439));
#6185=DIRECTION('',(-0.5,0.,0.866025403784439));
#6186=DIRECTION('center_axis',(0.,1.,0.));
#6187=DIRECTION('ref_axis',(1.,0.,0.));
#6188=DIRECTION('center_axis',(0.,-1.,0.));
#6189=DIRECTION('ref_axis',(0.,0.,-1.));
#6190=DIRECTION('center_axis',(0.,1.,0.));
#6191=DIRECTION('ref_axis',(1.,0.,0.));
#6192=DIRECTION('center_axis',(0.,1.,0.));
#6193=DIRECTION('ref_axis',(1.,0.,0.));
#6194=DIRECTION('center_axis',(0.,1.,0.));
#6195=DIRECTION('ref_axis',(0.,0.,1.));
#6196=DIRECTION('center_axis',(0.,-1.,0.));
#6197=DIRECTION('ref_axis',(1.,0.,0.));
#6198=DIRECTION('center_axis',(0.,-1.,0.));
#6199=DIRECTION('ref_axis',(1.,0.,0.));
#6200=DIRECTION('center_axis',(0.,-1.,0.));
#6201=DIRECTION('ref_axis',(1.,0.,0.));
#6202=DIRECTION('',(0.707106781186548,0.707106781186547,8.65956056235493E-17));
#6203=DIRECTION('center_axis',(0.,-1.,0.));
#6204=DIRECTION('ref_axis',(1.,0.,0.));
#6205=DIRECTION('center_axis',(0.,-1.,0.));
#6206=DIRECTION('ref_axis',(1.,0.,0.));
#6207=DIRECTION('',(0.,1.,0.));
#6208=DIRECTION('center_axis',(0.,1.,0.));
#6209=DIRECTION('ref_axis',(1.,0.,0.));
#6210=DIRECTION('center_axis',(0.,-1.,0.));
#6211=DIRECTION('ref_axis',(1.,0.,0.));
#6212=DIRECTION('',(-0.707106781186547,0.707106781186548,-8.65956056235493E-17));
#6213=DIRECTION('center_axis',(0.,-1.,0.));
#6214=DIRECTION('ref_axis',(0.,0.,-1.));
#6215=DIRECTION('center_axis',(0.,-1.,0.));
#6216=DIRECTION('ref_axis',(1.,0.,0.));
#6217=DIRECTION('center_axis',(0.,1.,0.));
#6218=DIRECTION('ref_axis',(1.,0.,0.));
#6219=DIRECTION('center_axis',(0.,1.,0.));
#6220=DIRECTION('ref_axis',(1.,0.,0.));
#6221=DIRECTION('',(-0.447213595499958,0.894427190999916,-5.47678698264203E-17));
#6222=DIRECTION('center_axis',(0.,-1.,0.));
#6223=DIRECTION('ref_axis',(1.,0.,0.));
#6224=DIRECTION('',(0.,1.,0.));
#6225=DIRECTION('axis',(0.,0.,1.));
#6226=DIRECTION('refdir',(1.,0.,0.));
#6227=DIRECTION('center_axis',(0.,0.,1.));
#6228=DIRECTION('ref_axis',(1.,0.,0.));
#6229=DIRECTION('center_axis',(0.,0.,1.));
#6230=DIRECTION('ref_axis',(1.,0.,0.));
#6231=DIRECTION('',(0.,0.,1.));
#6232=DIRECTION('center_axis',(0.,0.,-1.));
#6233=DIRECTION('ref_axis',(1.,0.,0.));
#6234=DIRECTION('center_axis',(0.,0.,1.));
#6235=DIRECTION('ref_axis',(1.,0.,0.));
#6236=DIRECTION('center_axis',(0.,0.,1.));
#6237=DIRECTION('ref_axis',(1.,0.,0.));
#6238=DIRECTION('center_axis',(0.,0.,1.));
#6239=DIRECTION('ref_axis',(1.,0.,0.));
#6240=DIRECTION('center_axis',(0.,0.,1.));
#6241=DIRECTION('ref_axis',(1.,0.,0.));
#6242=DIRECTION('',(0.,0.,1.));
#6243=DIRECTION('center_axis',(0.,0.,-1.));
#6244=DIRECTION('ref_axis',(1.,0.,0.));
#6245=DIRECTION('center_axis',(0.,0.,1.));
#6246=DIRECTION('ref_axis',(1.,0.,0.));
#6247=DIRECTION('center_axis',(0.,0.,1.));
#6248=DIRECTION('ref_axis',(1.,0.,0.));
#6249=DIRECTION('center_axis',(0.,0.,1.));
#6250=DIRECTION('ref_axis',(1.,0.,0.));
#6251=DIRECTION('center_axis',(0.,0.,1.));
#6252=DIRECTION('ref_axis',(1.,0.,0.));
#6253=DIRECTION('',(0.,0.,1.));
#6254=DIRECTION('center_axis',(0.,0.,1.));
#6255=DIRECTION('ref_axis',(1.,0.,0.));
#6256=DIRECTION('center_axis',(0.,0.,1.));
#6257=DIRECTION('ref_axis',(1.,0.,0.));
#6258=DIRECTION('',(0.,0.,1.));
#6259=DIRECTION('center_axis',(0.,1.,0.));
#6260=DIRECTION('ref_axis',(-1.,0.,0.));
#6261=DIRECTION('',(-1.,0.,0.));
#6262=DIRECTION('',(0.,0.,1.));
#6263=DIRECTION('',(-1.,0.,0.));
#6264=DIRECTION('',(0.,0.,1.));
#6265=DIRECTION('center_axis',(1.,0.,0.));
#6266=DIRECTION('ref_axis',(0.,1.,0.));
#6267=DIRECTION('',(0.,1.,0.));
#6268=DIRECTION('',(0.,1.,0.));
#6269=DIRECTION('',(0.,0.,1.));
#6270=DIRECTION('center_axis',(0.,-1.,0.));
#6271=DIRECTION('ref_axis',(1.,0.,0.));
#6272=DIRECTION('',(1.,0.,0.));
#6273=DIRECTION('',(1.,0.,0.));
#6274=DIRECTION('',(0.,0.,1.));
#6275=DIRECTION('center_axis',(-1.,0.,0.));
#6276=DIRECTION('ref_axis',(0.,-1.,0.));
#6277=DIRECTION('',(0.,-1.,0.));
#6278=DIRECTION('',(0.,-1.,0.));
#6279=DIRECTION('center_axis',(0.,0.,1.));
#6280=DIRECTION('ref_axis',(1.,0.,0.));
#6281=DIRECTION('center_axis',(0.,0.,1.));
#6282=DIRECTION('ref_axis',(1.,0.,0.));
#6283=DIRECTION('axis',(0.,0.,1.));
#6284=DIRECTION('refdir',(1.,0.,0.));
#6285=DIRECTION('center_axis',(0.,1.,0.));
#6286=DIRECTION('ref_axis',(-1.,0.,0.));
#6287=DIRECTION('',(-1.,0.,0.));
#6288=DIRECTION('',(0.,0.,1.));
#6289=DIRECTION('',(-1.,0.,0.));
#6290=DIRECTION('',(0.,0.,1.));
#6291=DIRECTION('center_axis',(1.,0.,0.));
#6292=DIRECTION('ref_axis',(0.,1.,0.));
#6293=DIRECTION('',(0.,1.,0.));
#6294=DIRECTION('',(0.,1.,0.));
#6295=DIRECTION('',(0.,0.,1.));
#6296=DIRECTION('center_axis',(0.,-1.,0.));
#6297=DIRECTION('ref_axis',(1.,0.,0.));
#6298=DIRECTION('',(1.,0.,0.));
#6299=DIRECTION('',(1.,0.,0.));
#6300=DIRECTION('',(0.,0.,1.));
#6301=DIRECTION('center_axis',(-1.,0.,0.));
#6302=DIRECTION('ref_axis',(0.,-1.,0.));
#6303=DIRECTION('',(0.,-1.,0.));
#6304=DIRECTION('',(0.,-1.,0.));
#6305=DIRECTION('center_axis',(0.,0.,1.));
#6306=DIRECTION('ref_axis',(1.,0.,0.));
#6307=DIRECTION('center_axis',(0.,0.,1.));
#6308=DIRECTION('ref_axis',(1.,0.,0.));
#6309=DIRECTION('axis',(0.,0.,1.));
#6310=DIRECTION('refdir',(1.,0.,0.));
#6311=DIRECTION('center_axis',(1.,0.,0.));
#6312=DIRECTION('ref_axis',(0.,0.,-1.));
#6313=DIRECTION('center_axis',(1.,0.,0.));
#6314=DIRECTION('ref_axis',(0.,0.,-1.));
#6315=DIRECTION('',(1.,0.,0.));
#6316=DIRECTION('center_axis',(-1.,0.,0.));
#6317=DIRECTION('ref_axis',(0.,0.,-1.));
#6318=DIRECTION('center_axis',(0.,0.,1.));
#6319=DIRECTION('ref_axis',(1.,0.,0.));
#6320=DIRECTION('center_axis',(0.,0.,1.));
#6321=DIRECTION('ref_axis',(1.,0.,0.));
#6322=DIRECTION('',(0.,0.,1.));
#6323=DIRECTION('center_axis',(0.,0.,-1.));
#6324=DIRECTION('ref_axis',(1.,0.,0.));
#6325=DIRECTION('center_axis',(0.,0.,1.));
#6326=DIRECTION('ref_axis',(1.,0.,0.));
#6327=DIRECTION('center_axis',(0.,0.,1.));
#6328=DIRECTION('ref_axis',(1.,0.,0.));
#6329=DIRECTION('',(0.,0.,1.));
#6330=DIRECTION('center_axis',(0.,0.,-1.));
#6331=DIRECTION('ref_axis',(1.,0.,0.));
#6332=DIRECTION('center_axis',(0.,0.,1.));
#6333=DIRECTION('ref_axis',(1.,0.,0.));
#6334=DIRECTION('center_axis',(0.,0.,1.));
#6335=DIRECTION('ref_axis',(1.,0.,0.));
#6336=DIRECTION('',(0.,0.,1.));
#6337=DIRECTION('center_axis',(0.,0.,-1.));
#6338=DIRECTION('ref_axis',(1.,0.,0.));
#6339=DIRECTION('center_axis',(0.,0.,1.));
#6340=DIRECTION('ref_axis',(1.,0.,0.));
#6341=DIRECTION('center_axis',(0.,0.,1.));
#6342=DIRECTION('ref_axis',(1.,0.,0.));
#6343=DIRECTION('',(0.,0.,1.));
#6344=DIRECTION('center_axis',(0.,0.,-1.));
#6345=DIRECTION('ref_axis',(1.,0.,0.));
#6346=DIRECTION('center_axis',(0.,0.,1.));
#6347=DIRECTION('ref_axis',(0.,-1.,0.));
#6348=DIRECTION('',(0.,-1.,0.));
#6349=DIRECTION('',(1.,0.,0.));
#6350=DIRECTION('',(0.,-1.,0.));
#6351=DIRECTION('',(1.,0.,0.));
#6352=DIRECTION('center_axis',(0.,1.,0.));
#6353=DIRECTION('ref_axis',(0.,0.,1.));
#6354=DIRECTION('',(0.,0.,1.));
#6355=DIRECTION('',(0.,0.,1.));
#6356=DIRECTION('',(1.,0.,0.));
#6357=DIRECTION('center_axis',(0.,-1.,0.));
#6358=DIRECTION('ref_axis',(0.,0.,-1.));
#6359=DIRECTION('',(0.,0.,-1.));
#6360=DIRECTION('',(-1.,0.,0.));
#6361=DIRECTION('',(0.,0.,-1.));
#6362=DIRECTION('center_axis',(1.,0.,0.));
#6363=DIRECTION('ref_axis',(0.,0.,-1.));
#6364=DIRECTION('',(0.,-1.,0.));
#6365=DIRECTION('center_axis',(1.,0.,0.));
#6366=DIRECTION('ref_axis',(0.,0.,-1.));
#6367=DIRECTION('',(0.,1.,0.));
#6368=DIRECTION('center_axis',(0.,1.,0.));
#6369=DIRECTION('ref_axis',(-1.,0.,0.));
#6370=DIRECTION('',(-1.,0.,0.));
#6371=DIRECTION('',(0.,0.,1.));
#6372=DIRECTION('',(-1.,0.,0.));
#6373=DIRECTION('',(0.,0.,1.));
#6374=DIRECTION('center_axis',(1.,0.,0.));
#6375=DIRECTION('ref_axis',(0.,1.,0.));
#6376=DIRECTION('',(0.,1.,0.));
#6377=DIRECTION('',(0.,1.,0.));
#6378=DIRECTION('',(0.,0.,1.));
#6379=DIRECTION('center_axis',(0.,-1.,0.));
#6380=DIRECTION('ref_axis',(1.,0.,0.));
#6381=DIRECTION('',(1.,0.,0.));
#6382=DIRECTION('',(1.,0.,0.));
#6383=DIRECTION('',(0.,0.,1.));
#6384=DIRECTION('center_axis',(-1.,0.,0.));
#6385=DIRECTION('ref_axis',(0.,-1.,0.));
#6386=DIRECTION('',(0.,-1.,0.));
#6387=DIRECTION('',(0.,-1.,0.));
#6388=DIRECTION('center_axis',(0.,0.,1.));
#6389=DIRECTION('ref_axis',(1.,0.,0.));
#6390=DIRECTION('center_axis',(0.,0.,1.));
#6391=DIRECTION('ref_axis',(1.,0.,0.));
#6392=DIRECTION('axis',(0.,0.,1.));
#6393=DIRECTION('refdir',(1.,0.,0.));
#6394=DIRECTION('center_axis',(0.866025403784439,0.,-0.5));
#6395=DIRECTION('ref_axis',(0.5,0.,0.866025403784439));
#6396=DIRECTION('',(-0.5,0.,-0.866025403784439));
#6397=DIRECTION('',(0.,-1.,0.));
#6398=DIRECTION('',(0.5,0.,0.866025403784439));
#6399=DIRECTION('',(0.,-1.,0.));
#6400=DIRECTION('center_axis',(1.20185167898973E-16,0.,-1.));
#6401=DIRECTION('ref_axis',(1.,0.,1.20185167898973E-16));
#6402=DIRECTION('',(-1.,0.,-1.20185167898973E-16));
#6403=DIRECTION('',(0.,-1.,0.));
#6404=DIRECTION('',(1.,0.,1.20185167898973E-16));
#6405=DIRECTION('center_axis',(-0.866025403784439,0.,-0.5));
#6406=DIRECTION('ref_axis',(0.5,0.,-0.866025403784439));
#6407=DIRECTION('',(-0.5,0.,0.866025403784439));
#6408=DIRECTION('',(0.,-1.,0.));
#6409=DIRECTION('',(0.5,0.,-0.866025403784439));
#6410=DIRECTION('center_axis',(-0.866025403784439,0.,0.5));
#6411=DIRECTION('ref_axis',(-0.5,0.,-0.866025403784439));
#6412=DIRECTION('',(0.5,0.,0.866025403784439));
#6413=DIRECTION('',(0.,-1.,0.));
#6414=DIRECTION('',(-0.5,0.,-0.866025403784439));
#6415=DIRECTION('center_axis',(-2.40370335797945E-16,0.,1.));
#6416=DIRECTION('ref_axis',(-1.,0.,-2.40370335797945E-16));
#6417=DIRECTION('',(1.,0.,2.40370335797945E-16));
#6418=DIRECTION('',(0.,-1.,0.));
#6419=DIRECTION('',(-1.,0.,-2.40370335797945E-16));
#6420=DIRECTION('center_axis',(0.866025403784439,0.,0.5));
#6421=DIRECTION('ref_axis',(-0.5,0.,0.866025403784439));
#6422=DIRECTION('',(0.5,0.,-0.866025403784439));
#6423=DIRECTION('',(-0.5,0.,0.866025403784439));
#6424=DIRECTION('center_axis',(0.,1.,0.));
#6425=DIRECTION('ref_axis',(1.,0.,0.));
#6426=DIRECTION('center_axis',(0.,-1.,0.));
#6427=DIRECTION('ref_axis',(0.,0.,-1.));
#6428=DIRECTION('center_axis',(0.,1.,0.));
#6429=DIRECTION('ref_axis',(1.,0.,0.));
#6430=DIRECTION('center_axis',(0.,1.,0.));
#6431=DIRECTION('ref_axis',(1.,0.,0.));
#6432=DIRECTION('center_axis',(0.,1.,0.));
#6433=DIRECTION('ref_axis',(0.,0.,1.));
#6434=DIRECTION('center_axis',(0.,-1.,0.));
#6435=DIRECTION('ref_axis',(1.,0.,0.));
#6436=DIRECTION('center_axis',(0.,-1.,0.));
#6437=DIRECTION('ref_axis',(1.,0.,0.));
#6438=DIRECTION('center_axis',(0.,-1.,0.));
#6439=DIRECTION('ref_axis',(1.,0.,0.));
#6440=DIRECTION('',(0.707106781186548,0.707106781186547,8.65956056235493E-17));
#6441=DIRECTION('center_axis',(0.,-1.,0.));
#6442=DIRECTION('ref_axis',(1.,0.,0.));
#6443=DIRECTION('center_axis',(0.,-1.,0.));
#6444=DIRECTION('ref_axis',(1.,0.,0.));
#6445=DIRECTION('',(0.,1.,0.));
#6446=DIRECTION('center_axis',(0.,1.,0.));
#6447=DIRECTION('ref_axis',(1.,0.,0.));
#6448=DIRECTION('center_axis',(0.,-1.,0.));
#6449=DIRECTION('ref_axis',(1.,0.,0.));
#6450=DIRECTION('',(-0.707106781186547,0.707106781186548,-8.65956056235493E-17));
#6451=DIRECTION('center_axis',(0.,-1.,0.));
#6452=DIRECTION('ref_axis',(0.,0.,-1.));
#6453=DIRECTION('center_axis',(0.,-1.,0.));
#6454=DIRECTION('ref_axis',(1.,0.,0.));
#6455=DIRECTION('center_axis',(0.,1.,0.));
#6456=DIRECTION('ref_axis',(1.,0.,0.));
#6457=DIRECTION('center_axis',(0.,1.,0.));
#6458=DIRECTION('ref_axis',(1.,0.,0.));
#6459=DIRECTION('',(-0.447213595499958,0.894427190999916,-5.47678698264203E-17));
#6460=DIRECTION('center_axis',(0.,-1.,0.));
#6461=DIRECTION('ref_axis',(1.,0.,0.));
#6462=DIRECTION('',(0.,1.,0.));
#6463=DIRECTION('axis',(0.,0.,1.));
#6464=DIRECTION('refdir',(1.,0.,0.));
#6465=DIRECTION('center_axis',(0.,-1.,0.));
#6466=DIRECTION('ref_axis',(1.,0.,0.));
#6467=DIRECTION('center_axis',(0.,1.,0.));
#6468=DIRECTION('ref_axis',(1.,0.,0.));
#6469=DIRECTION('',(0.,1.,0.));
#6470=DIRECTION('center_axis',(0.,-1.,0.));
#6471=DIRECTION('ref_axis',(1.,0.,0.));
#6472=DIRECTION('center_axis',(0.,1.,0.));
#6473=DIRECTION('ref_axis',(1.,0.,0.));
#6474=DIRECTION('center_axis',(0.,-1.,0.));
#6475=DIRECTION('ref_axis',(1.,0.,0.));
#6476=DIRECTION('',(-0.707106781186549,0.707106781186546,-8.65956056235496E-17));
#6477=DIRECTION('center_axis',(0.,-1.,0.));
#6478=DIRECTION('ref_axis',(0.,0.,-1.));
#6479=DIRECTION('center_axis',(0.,-1.,0.));
#6480=DIRECTION('ref_axis',(1.,0.,0.));
#6481=DIRECTION('center_axis',(0.,1.,0.));
#6482=DIRECTION('ref_axis',(1.,0.,0.));
#6483=DIRECTION('',(-0.866025403784439,-0.5,-1.06057523872491E-16));
#6484=DIRECTION('center_axis',(1.4792020664489E-16,0.,-1.));
#6485=DIRECTION('ref_axis',(-1.,0.,-1.4792020664489E-16));
#6486=DIRECTION('',(0.,1.,0.));
#6487=DIRECTION('',(-1.,0.,-1.4792020664489E-16));
#6488=DIRECTION('',(0.,1.,0.));
#6489=DIRECTION('center_axis',(0.866025403784439,0.,-0.5));
#6490=DIRECTION('ref_axis',(-0.5,0.,-0.866025403784439));
#6491=DIRECTION('',(0.,1.,0.));
#6492=DIRECTION('',(-0.5,0.,-0.866025403784439));
#6493=DIRECTION('center_axis',(0.866025403784439,0.,0.5));
#6494=DIRECTION('ref_axis',(0.5,0.,-0.866025403784439));
#6495=DIRECTION('',(0.,1.,0.));
#6496=DIRECTION('',(0.5,0.,-0.866025403784439));
#6497=DIRECTION('center_axis',(-2.95840413289779E-16,0.,1.));
#6498=DIRECTION('ref_axis',(1.,0.,2.95840413289779E-16));
#6499=DIRECTION('',(0.,1.,0.));
#6500=DIRECTION('',(1.,0.,2.95840413289779E-16));
#6501=DIRECTION('center_axis',(-0.866025403784439,0.,0.5));
#6502=DIRECTION('ref_axis',(0.5,0.,0.866025403784439));
#6503=DIRECTION('',(0.,1.,0.));
#6504=DIRECTION('',(0.5,0.,0.866025403784439));
#6505=DIRECTION('center_axis',(-0.866025403784439,0.,-0.5));
#6506=DIRECTION('ref_axis',(-0.5,0.,0.866025403784439));
#6507=DIRECTION('',(-0.5,0.,0.866025403784439));
#6508=DIRECTION('center_axis',(0.,1.,0.));
#6509=DIRECTION('ref_axis',(0.,0.,1.));
#6510=DIRECTION('center_axis',(0.,1.,0.));
#6511=DIRECTION('ref_axis',(1.,0.,0.));
#6512=DIRECTION('axis',(0.,0.,1.));
#6513=DIRECTION('refdir',(1.,0.,0.));
#6514=DIRECTION('center_axis',(0.,1.,0.));
#6515=DIRECTION('ref_axis',(1.,0.,0.));
#6516=DIRECTION('',(0.866025403784439,-0.5,1.06057523872491E-16));
#6517=DIRECTION('center_axis',(0.,-1.,0.));
#6518=DIRECTION('ref_axis',(1.,0.,0.));
#6519=DIRECTION('center_axis',(0.,-1.,0.));
#6520=DIRECTION('ref_axis',(1.,0.,0.));
#6521=DIRECTION('center_axis',(0.,1.,0.));
#6522=DIRECTION('ref_axis',(1.,0.,0.));
#6523=DIRECTION('',(-0.866025403784439,-0.5,-1.06057523872491E-16));
#6524=DIRECTION('center_axis',(1.4792020664489E-16,0.,-1.));
#6525=DIRECTION('ref_axis',(-1.,0.,-1.4792020664489E-16));
#6526=DIRECTION('',(0.,1.,0.));
#6527=DIRECTION('',(0.,1.,0.));
#6528=DIRECTION('center_axis',(-0.866025403784439,0.,-0.5));
#6529=DIRECTION('ref_axis',(-0.5,0.,0.866025403784439));
#6530=DIRECTION('',(0.,1.,0.));
#6531=DIRECTION('center_axis',(-0.866025403784439,0.,0.5));
#6532=DIRECTION('ref_axis',(0.5,0.,0.866025403784439));
#6533=DIRECTION('',(0.,1.,0.));
#6534=DIRECTION('center_axis',(0.,1.,0.));
#6535=DIRECTION('ref_axis',(1.,0.,0.));
#6536=DIRECTION('center_axis',(0.,1.,0.));
#6537=DIRECTION('ref_axis',(1.,0.,0.));
#6538=DIRECTION('',(0.,-1.,0.));
#6539=DIRECTION('center_axis',(0.,1.,0.));
#6540=DIRECTION('ref_axis',(1.,0.,0.));
#6541=DIRECTION('center_axis',(-2.95840413289779E-16,0.,1.));
#6542=DIRECTION('ref_axis',(1.,0.,2.95840413289779E-16));
#6543=DIRECTION('',(0.,1.,0.));
#6544=DIRECTION('center_axis',(0.866025403784439,0.,-0.5));
#6545=DIRECTION('ref_axis',(-0.5,0.,-0.866025403784439));
#6546=DIRECTION('',(0.,1.,0.));
#6547=DIRECTION('center_axis',(0.866025403784439,0.,0.5));
#6548=DIRECTION('ref_axis',(0.5,0.,-0.866025403784439));
#6549=DIRECTION('center_axis',(0.,1.,0.));
#6550=DIRECTION('ref_axis',(1.,0.,0.));
#6551=DIRECTION('center_axis',(0.,1.,0.));
#6552=DIRECTION('ref_axis',(1.,0.,0.));
#6553=DIRECTION('axis',(0.,0.,1.));
#6554=DIRECTION('refdir',(1.,0.,0.));
#6555=DIRECTION('center_axis',(-0.00107151163471255,0.0471293712697611,
0.998888219084865));
#6556=DIRECTION('ref_axis',(0.022704394310356,-0.998630154113891,0.0471415503931119));
#6557=DIRECTION('center_axis',(0.0010715115821705,0.0471293712204561,0.998888219087248));
#6558=DIRECTION('ref_axis',(0.234516922063796,-0.971043629832377,0.045564045339339));
#6559=DIRECTION('center_axis',(0.0010715115821705,0.0471293712204561,0.998888219087248));
#6560=DIRECTION('ref_axis',(0.234516922063796,-0.971043629832377,0.045564045339339));
#6561=DIRECTION('center_axis',(-0.00107151163471255,0.0471293712697611,
0.998888219084865));
#6562=DIRECTION('ref_axis',(0.022704394310356,-0.998630154113891,0.0471415503931119));
#6563=DIRECTION('axis',(0.,0.,1.));
#6564=DIRECTION('refdir',(1.,0.,0.));
#6565=DIRECTION('center_axis',(0.,0.,1.));
#6566=DIRECTION('ref_axis',(1.,0.,0.));
#6567=DIRECTION('',(0.,1.,0.));
#6568=DIRECTION('center_axis',(0.,0.,1.));
#6569=DIRECTION('ref_axis',(1.,0.,0.));
#6570=DIRECTION('center_axis',(0.,0.,1.));
#6571=DIRECTION('ref_axis',(1.,0.,0.));
#6572=DIRECTION('center_axis',(0.,0.,1.));
#6573=DIRECTION('ref_axis',(1.,0.,0.));
#6574=DIRECTION('',(0.,0.,1.));
#6575=DIRECTION('center_axis',(0.,0.,1.));
#6576=DIRECTION('ref_axis',(1.,0.,0.));
#6577=DIRECTION('center_axis',(0.,0.,1.));
#6578=DIRECTION('ref_axis',(1.,0.,0.));
#6579=DIRECTION('',(0.,-1.,0.));
#6580=DIRECTION('center_axis',(0.,1.,0.));
#6581=DIRECTION('ref_axis',(1.,0.,0.));
#6582=DIRECTION('center_axis',(0.,-1.,0.));
#6583=DIRECTION('ref_axis',(1.,0.,0.));
#6584=DIRECTION('',(0.,-1.,0.));
#6585=DIRECTION('center_axis',(0.,-1.,0.));
#6586=DIRECTION('ref_axis',(1.,0.,0.));
#6587=DIRECTION('center_axis',(0.,1.,0.));
#6588=DIRECTION('ref_axis',(1.,0.,0.));
#6589=DIRECTION('center_axis',(0.,1.,0.));
#6590=DIRECTION('ref_axis',(1.,0.,0.));
#6591=DIRECTION('',(0.,-1.,0.));
#6592=DIRECTION('center_axis',(0.,1.,0.));
#6593=DIRECTION('ref_axis',(1.,0.,0.));
#6594=DIRECTION('center_axis',(0.,1.,0.));
#6595=DIRECTION('ref_axis',(1.,0.,0.));
#6596=DIRECTION('center_axis',(0.,1.,0.));
#6597=DIRECTION('ref_axis',(1.,0.,0.));
#6598=DIRECTION('axis',(0.,0.,1.));
#6599=DIRECTION('refdir',(1.,0.,0.));
#6600=DIRECTION('center_axis',(0.866025403784439,0.,-0.5));
#6601=DIRECTION('ref_axis',(0.5,0.,0.866025403784439));
#6602=DIRECTION('',(0.5,0.,0.866025403784439));
#6603=DIRECTION('',(0.,-1.,0.));
#6604=DIRECTION('',(0.5,0.,0.866025403784439));
#6605=DIRECTION('',(0.,-1.,0.));
#6606=DIRECTION('center_axis',(1.92296268638356E-16,0.,-1.));
#6607=DIRECTION('ref_axis',(1.,0.,1.92296268638356E-16));
#6608=DIRECTION('',(1.,0.,1.92296268638356E-16));
#6609=DIRECTION('',(0.,-1.,0.));
#6610=DIRECTION('',(1.,0.,1.92296268638356E-16));
#6611=DIRECTION('center_axis',(-0.866025403784439,0.,-0.5));
#6612=DIRECTION('ref_axis',(0.5,0.,-0.866025403784439));
#6613=DIRECTION('',(0.5,0.,-0.866025403784439));
#6614=DIRECTION('',(0.,-1.,0.));
#6615=DIRECTION('',(0.5,0.,-0.866025403784438));
#6616=DIRECTION('center_axis',(-0.866025403784439,0.,0.5));
#6617=DIRECTION('ref_axis',(-0.5,0.,-0.866025403784439));
#6618=DIRECTION('',(-0.5,0.,-0.866025403784439));
#6619=DIRECTION('',(0.,-1.,0.));
#6620=DIRECTION('',(-0.5,0.,-0.866025403784439));
#6621=DIRECTION('center_axis',(-1.92296268638356E-16,0.,1.));
#6622=DIRECTION('ref_axis',(-1.,0.,-1.92296268638356E-16));
#6623=DIRECTION('',(-1.,0.,-1.92296268638356E-16));
#6624=DIRECTION('',(0.,-1.,0.));
#6625=DIRECTION('',(-1.,0.,-1.92296268638356E-16));
#6626=DIRECTION('center_axis',(0.866025403784439,0.,0.5));
#6627=DIRECTION('ref_axis',(-0.5,0.,0.866025403784439));
#6628=DIRECTION('',(-0.5,0.,0.866025403784439));
#6629=DIRECTION('',(-0.5,0.,0.866025403784439));
#6630=DIRECTION('center_axis',(0.,-1.,0.));
#6631=DIRECTION('ref_axis',(0.,0.,-1.));
#6632=DIRECTION('center_axis',(0.,1.,0.));
#6633=DIRECTION('ref_axis',(0.,0.,1.));
#6634=DIRECTION('center_axis',(0.,-1.,0.));
#6635=DIRECTION('ref_axis',(1.,0.,0.));
#6636=DIRECTION('center_axis',(0.,-1.,0.));
#6637=DIRECTION('ref_axis',(1.,0.,0.));
#6638=DIRECTION('center_axis',(0.,-1.,0.));
#6639=DIRECTION('ref_axis',(1.,0.,0.));
#6640=DIRECTION('',(0.707106781186547,0.707106781186548,8.65956056235493E-17));
#6641=DIRECTION('center_axis',(0.,-1.,0.));
#6642=DIRECTION('ref_axis',(1.,0.,0.));
#6643=DIRECTION('center_axis',(0.,1.,0.));
#6644=DIRECTION('ref_axis',(1.,0.,0.));
#6645=DIRECTION('',(0.,1.,0.));
#6646=DIRECTION('center_axis',(0.,1.,0.));
#6647=DIRECTION('ref_axis',(1.,0.,0.));
#6648=DIRECTION('center_axis',(0.,-1.,0.));
#6649=DIRECTION('ref_axis',(1.,0.,0.));
#6650=DIRECTION('',(-0.707106781186547,0.707106781186548,-8.65956056235493E-17));
#6651=DIRECTION('center_axis',(0.,-1.,0.));
#6652=DIRECTION('ref_axis',(0.,0.,-1.));
#6653=DIRECTION('axis',(0.,0.,1.));
#6654=DIRECTION('refdir',(1.,0.,0.));
#6655=DIRECTION('axis',(0.,0.,1.));
#6656=DIRECTION('refdir',(1.,0.,0.));
#6657=DIRECTION('center_axis',(1.,0.,0.));
#6658=DIRECTION('ref_axis',(0.,0.,-1.));
#6659=DIRECTION('center_axis',(1.,0.,0.));
#6660=DIRECTION('ref_axis',(0.,0.,-1.));
#6661=DIRECTION('',(1.,0.,0.));
#6662=DIRECTION('center_axis',(-1.,0.,0.));
#6663=DIRECTION('ref_axis',(0.,0.,-1.));
#6664=DIRECTION('center_axis',(1.,0.,0.));
#6665=DIRECTION('ref_axis',(0.,0.,-1.));
#6666=DIRECTION('center_axis',(1.,0.,0.));
#6667=DIRECTION('ref_axis',(0.,0.,-1.));
#6668=DIRECTION('',(1.,0.,0.));
#6669=DIRECTION('center_axis',(-1.,0.,0.));
#6670=DIRECTION('ref_axis',(0.,0.,-1.));
#6671=DIRECTION('center_axis',(1.,0.,0.));
#6672=DIRECTION('ref_axis',(0.,0.,-1.));
#6673=DIRECTION('center_axis',(1.,0.,0.));
#6674=DIRECTION('ref_axis',(0.,0.,-1.));
#6675=DIRECTION('',(1.,0.,0.));
#6676=DIRECTION('center_axis',(-1.,0.,0.));
#6677=DIRECTION('ref_axis',(0.,0.,-1.));
#6678=DIRECTION('center_axis',(1.,0.,0.));
#6679=DIRECTION('ref_axis',(0.,0.,-1.));
#6680=DIRECTION('center_axis',(1.,0.,0.));
#6681=DIRECTION('ref_axis',(0.,0.,-1.));
#6682=DIRECTION('',(1.,0.,0.));
#6683=DIRECTION('center_axis',(-1.,0.,0.));
#6684=DIRECTION('ref_axis',(0.,0.,-1.));
#6685=DIRECTION('center_axis',(0.,0.,1.));
#6686=DIRECTION('ref_axis',(1.,0.,0.));
#6687=DIRECTION('center_axis',(0.,0.,1.));
#6688=DIRECTION('ref_axis',(1.,0.,0.));
#6689=DIRECTION('',(0.,0.,1.));
#6690=DIRECTION('center_axis',(0.,0.,-1.));
#6691=DIRECTION('ref_axis',(1.,0.,0.));
#6692=DIRECTION('center_axis',(0.,0.,1.));
#6693=DIRECTION('ref_axis',(1.,0.,0.));
#6694=DIRECTION('center_axis',(0.,0.,1.));
#6695=DIRECTION('ref_axis',(1.,0.,0.));
#6696=DIRECTION('center_axis',(0.,0.,1.));
#6697=DIRECTION('ref_axis',(1.,0.,0.));
#6698=DIRECTION('',(0.,0.,1.));
#6699=DIRECTION('center_axis',(0.,0.,-1.));
#6700=DIRECTION('ref_axis',(1.,0.,0.));
#6701=DIRECTION('center_axis',(0.,0.,1.));
#6702=DIRECTION('ref_axis',(1.,0.,0.));
#6703=DIRECTION('center_axis',(0.,0.,1.));
#6704=DIRECTION('ref_axis',(1.,0.,0.));
#6705=DIRECTION('center_axis',(0.,0.,1.));
#6706=DIRECTION('ref_axis',(1.,0.,0.));
#6707=DIRECTION('',(0.,0.,1.));
#6708=DIRECTION('center_axis',(0.,0.,-1.));
#6709=DIRECTION('ref_axis',(1.,0.,0.));
#6710=DIRECTION('center_axis',(0.,0.,1.));
#6711=DIRECTION('ref_axis',(1.,0.,0.));
#6712=DIRECTION('center_axis',(0.,0.,1.));
#6713=DIRECTION('ref_axis',(1.,0.,0.));
#6714=DIRECTION('center_axis',(0.,0.,1.));
#6715=DIRECTION('ref_axis',(1.,0.,0.));
#6716=DIRECTION('',(0.,0.,1.));
#6717=DIRECTION('center_axis',(0.,0.,-1.));
#6718=DIRECTION('ref_axis',(1.,0.,0.));
#6719=DIRECTION('center_axis',(0.,0.,1.));
#6720=DIRECTION('ref_axis',(1.,0.,0.));
#6721=DIRECTION('center_axis',(1.,0.,0.));
#6722=DIRECTION('ref_axis',(0.,0.,-1.));
#6723=DIRECTION('center_axis',(1.,0.,0.));
#6724=DIRECTION('ref_axis',(0.,0.,-1.));
#6725=DIRECTION('',(1.,0.,0.));
#6726=DIRECTION('center_axis',(-1.,0.,0.));
#6727=DIRECTION('ref_axis',(0.,0.,-1.));
#6728=DIRECTION('center_axis',(1.,0.,0.));
#6729=DIRECTION('ref_axis',(0.,0.,-1.));
#6730=DIRECTION('center_axis',(1.,0.,0.));
#6731=DIRECTION('ref_axis',(0.,0.,-1.));
#6732=DIRECTION('',(1.,0.,0.));
#6733=DIRECTION('center_axis',(-1.,0.,0.));
#6734=DIRECTION('ref_axis',(0.,0.,-1.));
#6735=DIRECTION('center_axis',(0.,1.,0.));
#6736=DIRECTION('ref_axis',(-1.,0.,0.));
#6737=DIRECTION('',(-1.,0.,0.));
#6738=DIRECTION('',(0.,0.,1.));
#6739=DIRECTION('',(-1.,0.,0.));
#6740=DIRECTION('',(0.,0.,1.));
#6741=DIRECTION('center_axis',(1.,0.,0.));
#6742=DIRECTION('ref_axis',(0.,1.,0.));
#6743=DIRECTION('',(0.,1.,0.));
#6744=DIRECTION('',(0.,1.,0.));
#6745=DIRECTION('',(0.,0.,1.));
#6746=DIRECTION('center_axis',(0.,-1.,0.));
#6747=DIRECTION('ref_axis',(1.,0.,0.));
#6748=DIRECTION('',(1.,0.,0.));
#6749=DIRECTION('',(1.,0.,0.));
#6750=DIRECTION('',(0.,0.,1.));
#6751=DIRECTION('center_axis',(-1.,0.,0.));
#6752=DIRECTION('ref_axis',(0.,-1.,0.));
#6753=DIRECTION('',(0.,-1.,0.));
#6754=DIRECTION('',(0.,-1.,0.));
#6755=DIRECTION('center_axis',(0.,0.,1.));
#6756=DIRECTION('ref_axis',(1.,0.,0.));
#6757=DIRECTION('center_axis',(0.,0.,1.));
#6758=DIRECTION('ref_axis',(1.,0.,0.));
#6759=DIRECTION('axis',(0.,0.,1.));
#6760=DIRECTION('refdir',(1.,0.,0.));
#6761=DIRECTION('center_axis',(0.,0.,1.));
#6762=DIRECTION('ref_axis',(1.,0.,0.));
#6763=DIRECTION('center_axis',(0.,0.,1.));
#6764=DIRECTION('ref_axis',(1.,0.,0.));
#6765=DIRECTION('',(0.,0.,1.));
#6766=DIRECTION('center_axis',(0.,0.,-1.));
#6767=DIRECTION('ref_axis',(1.,0.,0.));
#6768=DIRECTION('center_axis',(0.,0.,1.));
#6769=DIRECTION('ref_axis',(1.,0.,0.));
#6770=DIRECTION('center_axis',(0.,0.,1.));
#6771=DIRECTION('ref_axis',(1.,0.,0.));
#6772=DIRECTION('',(0.,0.,1.));
#6773=DIRECTION('center_axis',(0.,0.,-1.));
#6774=DIRECTION('ref_axis',(1.,0.,0.));
#6775=DIRECTION('center_axis',(0.,0.,1.));
#6776=DIRECTION('ref_axis',(1.,0.,0.));
#6777=DIRECTION('center_axis',(0.,0.,1.));
#6778=DIRECTION('ref_axis',(1.,0.,0.));
#6779=DIRECTION('',(0.,0.,1.));
#6780=DIRECTION('center_axis',(0.,0.,-1.));
#6781=DIRECTION('ref_axis',(1.,0.,0.));
#6782=DIRECTION('center_axis',(0.,0.,1.));
#6783=DIRECTION('ref_axis',(1.,0.,0.));
#6784=DIRECTION('center_axis',(0.,0.,1.));
#6785=DIRECTION('ref_axis',(1.,0.,0.));
#6786=DIRECTION('',(0.,0.,1.));
#6787=DIRECTION('center_axis',(0.,0.,-1.));
#6788=DIRECTION('ref_axis',(1.,0.,0.));
#6789=DIRECTION('center_axis',(0.,0.,1.));
#6790=DIRECTION('ref_axis',(1.,0.,0.));
#6791=DIRECTION('center_axis',(0.,0.,1.));
#6792=DIRECTION('ref_axis',(1.,0.,0.));
#6793=DIRECTION('',(0.,0.,1.));
#6794=DIRECTION('center_axis',(0.,0.,-1.));
#6795=DIRECTION('ref_axis',(1.,0.,0.));
#6796=DIRECTION('center_axis',(0.,1.,0.));
#6797=DIRECTION('ref_axis',(-1.,0.,0.));
#6798=DIRECTION('',(-1.,0.,0.));
#6799=DIRECTION('',(0.,0.,1.));
#6800=DIRECTION('',(-1.,0.,0.));
#6801=DIRECTION('',(0.,0.,1.));
#6802=DIRECTION('center_axis',(1.,0.,0.));
#6803=DIRECTION('ref_axis',(0.,1.,0.));
#6804=DIRECTION('',(0.,1.,0.));
#6805=DIRECTION('',(0.,1.,0.));
#6806=DIRECTION('',(0.,0.,1.));
#6807=DIRECTION('center_axis',(0.,-1.,0.));
#6808=DIRECTION('ref_axis',(1.,0.,0.));
#6809=DIRECTION('',(1.,0.,0.));
#6810=DIRECTION('',(1.,0.,0.));
#6811=DIRECTION('',(0.,0.,1.));
#6812=DIRECTION('center_axis',(-1.,0.,0.));
#6813=DIRECTION('ref_axis',(0.,-1.,0.));
#6814=DIRECTION('',(0.,-1.,0.));
#6815=DIRECTION('',(0.,-1.,0.));
#6816=DIRECTION('center_axis',(0.,0.,1.));
#6817=DIRECTION('ref_axis',(1.,0.,0.));
#6818=DIRECTION('center_axis',(0.,0.,1.));
#6819=DIRECTION('ref_axis',(1.,0.,0.));
#6820=DIRECTION('axis',(0.,0.,1.));
#6821=DIRECTION('refdir',(1.,0.,0.));
#6822=DIRECTION('axis',(0.,0.,1.));
#6823=DIRECTION('refdir',(1.,0.,0.));
#6824=DIRECTION('center_axis',(0.,1.,0.));
#6825=DIRECTION('ref_axis',(0.,0.,1.));
#6826=DIRECTION('center_axis',(0.,-1.,0.));
#6827=DIRECTION('ref_axis',(1.,0.,0.));
#6828=DIRECTION('',(-1.,0.,0.));
#6829=DIRECTION('',(0.,0.,-1.));
#6830=DIRECTION('',(1.,0.,0.));
#6831=DIRECTION('center_axis',(0.,0.,1.));
#6832=DIRECTION('ref_axis',(1.,0.,0.));
#6833=DIRECTION('',(0.,-1.,0.));
#6834=DIRECTION('',(0.,1.,0.));
#6835=DIRECTION('',(-1.,0.,0.));
#6836=DIRECTION('center_axis',(0.,-1.,0.));
#6837=DIRECTION('ref_axis',(0.,0.,-1.));
#6838=DIRECTION('center_axis',(0.,1.,0.));
#6839=DIRECTION('ref_axis',(1.,0.,0.));
#6840=DIRECTION('',(0.,0.,1.));
#6841=DIRECTION('',(1.,0.,0.));
#6842=DIRECTION('center_axis',(0.,0.,-1.));
#6843=DIRECTION('ref_axis',(-1.,0.,0.));
#6844=DIRECTION('',(0.,1.,0.));
#6845=DIRECTION('',(0.,1.,0.));
#6846=DIRECTION('center_axis',(1.,0.,0.));
#6847=DIRECTION('ref_axis',(0.,0.,-1.));
#6848=DIRECTION('center_axis',(0.,1.,0.));
#6849=DIRECTION('ref_axis',(0.,0.,1.));
#6850=DIRECTION('center_axis',(0.,-1.,0.));
#6851=DIRECTION('ref_axis',(1.,0.,0.));
#6852=DIRECTION('center_axis',(0.,-1.,0.));
#6853=DIRECTION('ref_axis',(1.,0.,0.));
#6854=DIRECTION('center_axis',(0.,-1.,0.));
#6855=DIRECTION('ref_axis',(1.,0.,0.));
#6856=DIRECTION('center_axis',(0.,-1.,0.));
#6857=DIRECTION('ref_axis',(1.,0.,0.));
#6858=DIRECTION('',(0.,1.,0.));
#6859=DIRECTION('center_axis',(0.,-1.,0.));
#6860=DIRECTION('ref_axis',(0.,0.,-1.));
#6861=DIRECTION('center_axis',(0.,-1.,0.));
#6862=DIRECTION('ref_axis',(1.,0.,0.));
#6863=DIRECTION('center_axis',(0.,-1.,0.));
#6864=DIRECTION('ref_axis',(1.,0.,0.));
#6865=DIRECTION('center_axis',(0.,-1.,0.));
#6866=DIRECTION('ref_axis',(1.,0.,0.));
#6867=DIRECTION('',(0.,1.,0.));
#6868=DIRECTION('center_axis',(0.,1.,0.));
#6869=DIRECTION('ref_axis',(0.,0.,1.));
#6870=DIRECTION('center_axis',(0.,-1.,0.));
#6871=DIRECTION('ref_axis',(1.,0.,0.));
#6872=DIRECTION('center_axis',(0.,-1.,0.));
#6873=DIRECTION('ref_axis',(1.,0.,0.));
#6874=DIRECTION('center_axis',(0.,-1.,0.));
#6875=DIRECTION('ref_axis',(1.,0.,0.));
#6876=DIRECTION('',(0.,1.,0.));
#6877=DIRECTION('center_axis',(0.,-1.,0.));
#6878=DIRECTION('ref_axis',(0.,0.,-1.));
#6879=DIRECTION('center_axis',(0.,-1.,0.));
#6880=DIRECTION('ref_axis',(1.,0.,0.));
#6881=DIRECTION('center_axis',(0.,-1.,0.));
#6882=DIRECTION('ref_axis',(1.,0.,0.));
#6883=DIRECTION('center_axis',(0.,-1.,0.));
#6884=DIRECTION('ref_axis',(1.,0.,0.));
#6885=DIRECTION('',(0.,1.,0.));
#6886=DIRECTION('center_axis',(0.,1.,0.));
#6887=DIRECTION('ref_axis',(0.,0.,1.));
#6888=DIRECTION('center_axis',(0.,-1.,0.));
#6889=DIRECTION('ref_axis',(1.,0.,0.));
#6890=DIRECTION('center_axis',(0.,-1.,0.));
#6891=DIRECTION('ref_axis',(1.,0.,0.));
#6892=DIRECTION('center_axis',(0.,-1.,0.));
#6893=DIRECTION('ref_axis',(1.,0.,0.));
#6894=DIRECTION('',(0.,1.,0.));
#6895=DIRECTION('center_axis',(0.,-1.,0.));
#6896=DIRECTION('ref_axis',(0.,0.,-1.));
#6897=DIRECTION('center_axis',(0.,-1.,0.));
#6898=DIRECTION('ref_axis',(1.,0.,0.));
#6899=DIRECTION('center_axis',(0.,-1.,0.));
#6900=DIRECTION('ref_axis',(1.,0.,0.));
#6901=DIRECTION('',(0.,1.,0.));
#6902=DIRECTION('axis',(0.,0.,1.));
#6903=DIRECTION('refdir',(1.,0.,0.));
#6904=DIRECTION('center_axis',(0.,1.,0.));
#6905=DIRECTION('ref_axis',(0.,0.,1.));
#6906=DIRECTION('center_axis',(0.,1.,0.));
#6907=DIRECTION('ref_axis',(1.,0.,0.));
#6908=DIRECTION('',(1.,0.,0.));
#6909=DIRECTION('center_axis',(0.,-1.,0.));
#6910=DIRECTION('ref_axis',(1.,0.,0.));
#6911=DIRECTION('',(-1.,0.,0.));
#6912=DIRECTION('center_axis',(0.,0.,-1.));
#6913=DIRECTION('ref_axis',(-1.,0.,0.));
#6914=DIRECTION('',(0.,-1.,0.));
#6915=DIRECTION('',(0.,1.,0.));
#6916=DIRECTION('',(1.,0.,0.));
#6917=DIRECTION('center_axis',(0.,-1.,0.));
#6918=DIRECTION('ref_axis',(0.,0.,-1.));
#6919=DIRECTION('center_axis',(0.,-1.,0.));
#6920=DIRECTION('ref_axis',(1.,0.,0.));
#6921=DIRECTION('center_axis',(0.,1.,0.));
#6922=DIRECTION('ref_axis',(1.,0.,0.));
#6923=DIRECTION('',(-1.,0.,0.));
#6924=DIRECTION('center_axis',(0.,0.,1.));
#6925=DIRECTION('ref_axis',(1.,0.,0.));
#6926=DIRECTION('',(0.,1.,0.));
#6927=DIRECTION('',(0.,-1.,0.));
#6928=DIRECTION('center_axis',(0.,1.,0.));
#6929=DIRECTION('ref_axis',(0.,0.,1.));
#6930=DIRECTION('center_axis',(0.,-1.,0.));
#6931=DIRECTION('ref_axis',(1.,0.,0.));
#6932=DIRECTION('center_axis',(0.,-1.,0.));
#6933=DIRECTION('ref_axis',(1.,0.,0.));
#6934=DIRECTION('center_axis',(0.,-1.,0.));
#6935=DIRECTION('ref_axis',(1.,0.,0.));
#6936=DIRECTION('center_axis',(0.,-1.,0.));
#6937=DIRECTION('ref_axis',(1.,0.,0.));
#6938=DIRECTION('',(0.,1.,0.));
#6939=DIRECTION('center_axis',(0.,-1.,0.));
#6940=DIRECTION('ref_axis',(0.,0.,-1.));
#6941=DIRECTION('center_axis',(0.,-1.,0.));
#6942=DIRECTION('ref_axis',(1.,0.,0.));
#6943=DIRECTION('center_axis',(0.,-1.,0.));
#6944=DIRECTION('ref_axis',(1.,0.,0.));
#6945=DIRECTION('',(0.,1.,0.));
#6946=DIRECTION('',(0.,0.,1.));
#6947=DIRECTION('',(1.,0.,0.));
#6948=DIRECTION('',(0.,0.,1.));
#6949=DIRECTION('',(1.,0.,0.));
#6950=DIRECTION('axis',(0.,0.,1.));
#6951=DIRECTION('refdir',(1.,0.,0.));
#6952=DIRECTION('center_axis',(1.,0.,0.));
#6953=DIRECTION('ref_axis',(0.,0.,-1.));
#6954=DIRECTION('center_axis',(1.,0.,0.));
#6955=DIRECTION('ref_axis',(0.,0.,-1.));
#6956=DIRECTION('',(1.,0.,0.));
#6957=DIRECTION('center_axis',(-1.,0.,0.));
#6958=DIRECTION('ref_axis',(0.,0.,-1.));
#6959=DIRECTION('center_axis',(1.,0.,0.));
#6960=DIRECTION('ref_axis',(0.,0.,-1.));
#6961=DIRECTION('center_axis',(1.,0.,0.));
#6962=DIRECTION('ref_axis',(0.,0.,-1.));
#6963=DIRECTION('',(1.,0.,0.));
#6964=DIRECTION('center_axis',(-1.,0.,0.));
#6965=DIRECTION('ref_axis',(0.,0.,-1.));
#6966=DIRECTION('center_axis',(1.,0.,0.));
#6967=DIRECTION('ref_axis',(0.,0.,-1.));
#6968=DIRECTION('center_axis',(1.,0.,0.));
#6969=DIRECTION('ref_axis',(0.,0.,-1.));
#6970=DIRECTION('',(1.,0.,0.));
#6971=DIRECTION('center_axis',(-1.,0.,0.));
#6972=DIRECTION('ref_axis',(0.,0.,-1.));
#6973=DIRECTION('center_axis',(1.,0.,0.));
#6974=DIRECTION('ref_axis',(0.,0.,-1.));
#6975=DIRECTION('center_axis',(1.,0.,0.));
#6976=DIRECTION('ref_axis',(0.,0.,-1.));
#6977=DIRECTION('',(1.,0.,0.));
#6978=DIRECTION('center_axis',(-1.,0.,0.));
#6979=DIRECTION('ref_axis',(0.,0.,-1.));
#6980=DIRECTION('center_axis',(1.,0.,0.));
#6981=DIRECTION('ref_axis',(0.,0.,-1.));
#6982=DIRECTION('center_axis',(1.,0.,0.));
#6983=DIRECTION('ref_axis',(0.,0.,-1.));
#6984=DIRECTION('',(1.,0.,0.));
#6985=DIRECTION('center_axis',(-1.,0.,0.));
#6986=DIRECTION('ref_axis',(0.,0.,-1.));
#6987=DIRECTION('center_axis',(1.,0.,0.));
#6988=DIRECTION('ref_axis',(0.,0.,-1.));
#6989=DIRECTION('center_axis',(1.,0.,0.));
#6990=DIRECTION('ref_axis',(0.,0.,-1.));
#6991=DIRECTION('',(1.,0.,0.));
#6992=DIRECTION('center_axis',(-1.,0.,0.));
#6993=DIRECTION('ref_axis',(0.,0.,-1.));
#6994=DIRECTION('center_axis',(0.,1.,0.));
#6995=DIRECTION('ref_axis',(-1.,0.,0.));
#6996=DIRECTION('',(-1.,0.,0.));
#6997=DIRECTION('',(0.,0.,1.));
#6998=DIRECTION('',(-1.,0.,0.));
#6999=DIRECTION('',(0.,0.,1.));
#7000=DIRECTION('center_axis',(1.,0.,0.));
#7001=DIRECTION('ref_axis',(0.,1.,0.));
#7002=DIRECTION('',(0.,1.,0.));
#7003=DIRECTION('',(0.,1.,0.));
#7004=DIRECTION('',(0.,0.,1.));
#7005=DIRECTION('center_axis',(0.,-1.,0.));
#7006=DIRECTION('ref_axis',(1.,0.,0.));
#7007=DIRECTION('',(1.,0.,0.));
#7008=DIRECTION('',(1.,0.,0.));
#7009=DIRECTION('',(0.,0.,1.));
#7010=DIRECTION('center_axis',(-1.,0.,0.));
#7011=DIRECTION('ref_axis',(0.,-1.,0.));
#7012=DIRECTION('',(0.,-1.,0.));
#7013=DIRECTION('',(0.,-1.,0.));
#7014=DIRECTION('center_axis',(0.,0.,1.));
#7015=DIRECTION('ref_axis',(1.,0.,0.));
#7016=DIRECTION('center_axis',(0.,0.,1.));
#7017=DIRECTION('ref_axis',(1.,0.,0.));
#7018=DIRECTION('axis',(0.,0.,1.));
#7019=DIRECTION('refdir',(1.,0.,0.));
#7020=DIRECTION('center_axis',(0.,1.,0.));
#7021=DIRECTION('ref_axis',(0.,0.,1.));
#7022=DIRECTION('center_axis',(0.,-1.,0.));
#7023=DIRECTION('ref_axis',(1.,0.,0.));
#7024=DIRECTION('center_axis',(0.,-1.,0.));
#7025=DIRECTION('ref_axis',(1.,0.,0.));
#7026=DIRECTION('center_axis',(0.,-1.,0.));
#7027=DIRECTION('ref_axis',(1.,0.,0.));
#7028=DIRECTION('',(0.707106781186547,0.707106781186548,8.65956056235493E-17));
#7029=DIRECTION('center_axis',(0.,-1.,0.));
#7030=DIRECTION('ref_axis',(1.,0.,0.));
#7031=DIRECTION('center_axis',(0.,-1.,0.));
#7032=DIRECTION('ref_axis',(1.,0.,0.));
#7033=DIRECTION('',(0.,1.,0.));
#7034=DIRECTION('center_axis',(0.,1.,0.));
#7035=DIRECTION('ref_axis',(1.,0.,0.));
#7036=DIRECTION('center_axis',(0.,-1.,0.));
#7037=DIRECTION('ref_axis',(1.,0.,0.));
#7038=DIRECTION('',(-0.707106781186547,0.707106781186548,-8.65956056235493E-17));
#7039=DIRECTION('center_axis',(0.,-1.,0.));
#7040=DIRECTION('ref_axis',(0.,0.,-1.));
#7041=DIRECTION('center_axis',(0.,-1.,0.));
#7042=DIRECTION('ref_axis',(1.,0.,0.));
#7043=DIRECTION('center_axis',(0.,1.,0.));
#7044=DIRECTION('ref_axis',(1.,0.,0.));
#7045=DIRECTION('center_axis',(0.,1.,0.));
#7046=DIRECTION('ref_axis',(1.,0.,0.));
#7047=DIRECTION('',(-0.447213595499958,0.894427190999916,-5.47678698264203E-17));
#7048=DIRECTION('center_axis',(0.,-1.,0.));
#7049=DIRECTION('ref_axis',(1.,0.,0.));
#7050=DIRECTION('center_axis',(0.,1.,0.));
#7051=DIRECTION('ref_axis',(1.,0.,0.));
#7052=DIRECTION('',(0.,1.,0.));
#7053=DIRECTION('center_axis',(0.,1.,0.));
#7054=DIRECTION('ref_axis',(1.,0.,0.));
#7055=DIRECTION('center_axis',(0.,-1.,0.));
#7056=DIRECTION('ref_axis',(1.,0.,0.));
#7057=DIRECTION('',(-0.707106781186547,0.707106781186548,-8.65956056235493E-17));
#7058=DIRECTION('center_axis',(0.,-1.,0.));
#7059=DIRECTION('ref_axis',(0.,0.,-1.));
#7060=DIRECTION('center_axis',(0.866025403784439,0.,-0.5));
#7061=DIRECTION('ref_axis',(0.5,0.,0.866025403784439));
#7062=DIRECTION('',(-0.5,0.,-0.866025403784439));
#7063=DIRECTION('',(0.,-1.,0.));
#7064=DIRECTION('',(0.5,0.,0.866025403784439));
#7065=DIRECTION('',(0.,-1.,0.));
#7066=DIRECTION('center_axis',(1.60246890531964E-16,0.,-1.));
#7067=DIRECTION('ref_axis',(1.,0.,1.60246890531964E-16));
#7068=DIRECTION('',(-1.,0.,-1.60246890531964E-16));
#7069=DIRECTION('',(0.,-1.,0.));
#7070=DIRECTION('',(1.,0.,1.60246890531964E-16));
#7071=DIRECTION('center_axis',(-0.866025403784439,0.,-0.5));
#7072=DIRECTION('ref_axis',(0.5,0.,-0.866025403784439));
#7073=DIRECTION('',(-0.5,0.,0.866025403784439));
#7074=DIRECTION('',(0.,-1.,0.));
#7075=DIRECTION('',(0.5,0.,-0.866025403784439));
#7076=DIRECTION('center_axis',(-0.866025403784439,0.,0.5));
#7077=DIRECTION('ref_axis',(-0.5,0.,-0.866025403784439));
#7078=DIRECTION('',(0.5,0.,0.866025403784439));
#7079=DIRECTION('',(0.,-1.,0.));
#7080=DIRECTION('',(-0.5,0.,-0.866025403784439));
#7081=DIRECTION('center_axis',(-1.60246890531964E-16,0.,1.));
#7082=DIRECTION('ref_axis',(-1.,0.,-1.60246890531964E-16));
#7083=DIRECTION('',(1.,0.,1.60246890531964E-16));
#7084=DIRECTION('',(0.,-1.,0.));
#7085=DIRECTION('',(-1.,0.,-1.60246890531964E-16));
#7086=DIRECTION('center_axis',(0.866025403784439,0.,0.5));
#7087=DIRECTION('ref_axis',(-0.5,0.,0.866025403784439));
#7088=DIRECTION('',(0.5,0.,-0.866025403784439));
#7089=DIRECTION('',(-0.5,0.,0.866025403784439));
#7090=DIRECTION('center_axis',(0.,1.,0.));
#7091=DIRECTION('ref_axis',(1.,0.,0.));
#7092=DIRECTION('center_axis',(0.,-1.,0.));
#7093=DIRECTION('ref_axis',(0.,0.,-1.));
#7094=DIRECTION('axis',(0.,0.,1.));
#7095=DIRECTION('refdir',(1.,0.,0.));
#7096=DIRECTION('center_axis',(0.,1.,0.));
#7097=DIRECTION('ref_axis',(0.,0.,1.));
#7098=DIRECTION('center_axis',(0.,-1.,0.));
#7099=DIRECTION('ref_axis',(1.,0.,0.));
#7100=DIRECTION('center_axis',(0.,-1.,0.));
#7101=DIRECTION('ref_axis',(1.,0.,0.));
#7102=DIRECTION('center_axis',(0.,-1.,0.));
#7103=DIRECTION('ref_axis',(1.,0.,0.));
#7104=DIRECTION('',(0.707106781186548,0.707106781186547,8.65956056235493E-17));
#7105=DIRECTION('center_axis',(0.,-1.,0.));
#7106=DIRECTION('ref_axis',(1.,0.,0.));
#7107=DIRECTION('center_axis',(0.,-1.,0.));
#7108=DIRECTION('ref_axis',(1.,0.,0.));
#7109=DIRECTION('',(0.,1.,0.));
#7110=DIRECTION('center_axis',(0.,1.,0.));
#7111=DIRECTION('ref_axis',(1.,0.,0.));
#7112=DIRECTION('center_axis',(0.,-1.,0.));
#7113=DIRECTION('ref_axis',(1.,0.,0.));
#7114=DIRECTION('',(-0.707106781186547,0.707106781186548,-8.65956056235493E-17));
#7115=DIRECTION('center_axis',(0.,-1.,0.));
#7116=DIRECTION('ref_axis',(0.,0.,-1.));
#7117=DIRECTION('center_axis',(0.,-1.,0.));
#7118=DIRECTION('ref_axis',(1.,0.,0.));
#7119=DIRECTION('center_axis',(0.,1.,0.));
#7120=DIRECTION('ref_axis',(1.,0.,0.));
#7121=DIRECTION('center_axis',(0.,1.,0.));
#7122=DIRECTION('ref_axis',(1.,0.,0.));
#7123=DIRECTION('',(-0.447213595499958,0.894427190999916,-5.47678698264203E-17));
#7124=DIRECTION('center_axis',(0.,-1.,0.));
#7125=DIRECTION('ref_axis',(1.,0.,0.));
#7126=DIRECTION('center_axis',(0.,1.,0.));
#7127=DIRECTION('ref_axis',(1.,0.,0.));
#7128=DIRECTION('',(0.,1.,0.));
#7129=DIRECTION('center_axis',(0.,1.,0.));
#7130=DIRECTION('ref_axis',(1.,0.,0.));
#7131=DIRECTION('center_axis',(0.,-1.,0.));
#7132=DIRECTION('ref_axis',(1.,0.,0.));
#7133=DIRECTION('',(-0.707106781186547,0.707106781186548,-8.65956056235493E-17));
#7134=DIRECTION('center_axis',(0.,-1.,0.));
#7135=DIRECTION('ref_axis',(0.,0.,-1.));
#7136=DIRECTION('center_axis',(0.866025403784439,0.,-0.5));
#7137=DIRECTION('ref_axis',(0.5,0.,0.866025403784439));
#7138=DIRECTION('',(-0.5,0.,-0.866025403784439));
#7139=DIRECTION('',(0.,-1.,0.));
#7140=DIRECTION('',(0.5,0.,0.866025403784439));
#7141=DIRECTION('',(0.,-1.,0.));
#7142=DIRECTION('center_axis',(1.20185167898973E-16,0.,-1.));
#7143=DIRECTION('ref_axis',(1.,0.,1.20185167898973E-16));
#7144=DIRECTION('',(-1.,0.,-1.20185167898973E-16));
#7145=DIRECTION('',(0.,-1.,0.));
#7146=DIRECTION('',(1.,0.,1.20185167898973E-16));
#7147=DIRECTION('center_axis',(-0.866025403784439,0.,-0.5));
#7148=DIRECTION('ref_axis',(0.5,0.,-0.866025403784439));
#7149=DIRECTION('',(-0.5,0.,0.866025403784439));
#7150=DIRECTION('',(0.,-1.,0.));
#7151=DIRECTION('',(0.5,0.,-0.866025403784439));
#7152=DIRECTION('center_axis',(-0.866025403784439,0.,0.5));
#7153=DIRECTION('ref_axis',(-0.5,0.,-0.866025403784439));
#7154=DIRECTION('',(0.5,0.,0.866025403784439));
#7155=DIRECTION('',(0.,-1.,0.));
#7156=DIRECTION('',(-0.5,0.,-0.866025403784439));
#7157=DIRECTION('center_axis',(-2.40370335797945E-16,0.,1.));
#7158=DIRECTION('ref_axis',(-1.,0.,-2.40370335797945E-16));
#7159=DIRECTION('',(1.,0.,2.40370335797945E-16));
#7160=DIRECTION('',(0.,-1.,0.));
#7161=DIRECTION('',(-1.,0.,-2.40370335797945E-16));
#7162=DIRECTION('center_axis',(0.866025403784439,0.,0.5));
#7163=DIRECTION('ref_axis',(-0.5,0.,0.866025403784439));
#7164=DIRECTION('',(0.5,0.,-0.866025403784439));
#7165=DIRECTION('',(-0.5,0.,0.866025403784439));
#7166=DIRECTION('center_axis',(0.,1.,0.));
#7167=DIRECTION('ref_axis',(1.,0.,0.));
#7168=DIRECTION('center_axis',(0.,-1.,0.));
#7169=DIRECTION('ref_axis',(0.,0.,-1.));
#7170=DIRECTION('',(0.,0.,1.));
#7171=DIRECTION('',(1.,0.,0.));
#7172=DIRECTION('',(0.,0.,1.));
#7173=DIRECTION('',(1.,0.,0.));
#7174=DIRECTION('',(0.,0.,1.));
#7175=DIRECTION('',(2.22044604925031E-16,-1.,0.));
#7176=DIRECTION('',(0.,-1.,2.22044604925031E-16));
#7177=DIRECTION('',(1.,0.,0.));
#7178=DIRECTION('',(0.,-1.,2.22044604925031E-16));
#7179=DIRECTION('',(1.,0.,0.));
#7180=DIRECTION('',(0.,0.,1.));
#7181=DIRECTION('',(-1.,1.22464679914735E-16,0.));
#7182=DIRECTION('',(0.,0.,1.));
#7183=DIRECTION('',(2.22044604925031E-16,-1.,0.));
#7184=DIRECTION('',(0.,-1.,2.22044604925031E-16));
#7185=DIRECTION('',(1.,0.,0.));
#7186=DIRECTION('',(0.,-1.,2.22044604925031E-16));
#7187=DIRECTION('',(1.,0.,0.));
#7188=DIRECTION('',(0.,0.,1.));
#7189=DIRECTION('',(-1.,1.22464679914735E-16,0.));
#7190=DIRECTION('',(0.,0.,1.));
#7191=DIRECTION('',(1.,0.,0.));
#7192=DIRECTION('',(0.,0.,1.));
#7193=DIRECTION('',(2.22044604925031E-16,-1.,0.));
#7194=DIRECTION('',(0.,-1.,2.22044604925031E-16));
#7195=DIRECTION('',(1.,0.,0.));
#7196=DIRECTION('',(0.,-1.,2.22044604925031E-16));
#7197=DIRECTION('',(1.,0.,0.));
#7198=DIRECTION('',(0.,0.,1.));
#7199=DIRECTION('',(-1.,1.22464679914735E-16,0.));
#7200=DIRECTION('',(0.,0.,1.));
#7201=DIRECTION('',(2.22044604925031E-16,-1.,0.));
#7202=DIRECTION('',(0.,-1.,2.22044604925031E-16));
#7203=DIRECTION('',(1.,0.,0.));
#7204=DIRECTION('',(0.,-1.,2.22044604925031E-16));
#7205=DIRECTION('',(1.,0.,0.));
#7206=DIRECTION('',(0.,0.,1.));
#7207=DIRECTION('',(-1.,1.22464679914735E-16,0.));
#7208=DIRECTION('',(0.,0.,1.));
#7209=DIRECTION('',(1.,0.,0.));
#7210=DIRECTION('',(0.,-1.,2.22044604925031E-16));
#7211=DIRECTION('',(1.,0.,0.));
#7212=DIRECTION('',(0.,-1.,2.22044604925031E-16));
#7213=DIRECTION('',(1.,0.,0.));
#7214=DIRECTION('',(0.,0.,1.));
#7215=DIRECTION('',(1.,0.,0.));
#7216=DIRECTION('',(0.,-1.,2.22044604925031E-16));
#7217=DIRECTION('',(1.,0.,0.));
#7218=DIRECTION('',(0.,-1.,2.22044604925031E-16));
#7219=DIRECTION('',(1.,0.,0.));
#7220=DIRECTION('',(0.,0.,1.));
#7221=DIRECTION('',(1.,0.,0.));
#7222=DIRECTION('',(0.,0.,1.));
#7223=DIRECTION('',(1.,0.,0.));
#7224=DIRECTION('',(0.,0.,1.));
#7225=DIRECTION('',(1.,0.,0.));
#7226=DIRECTION('',(0.,-1.,2.22044604925031E-16));
#7227=DIRECTION('',(1.,0.,0.));
#7228=DIRECTION('',(0.,-1.,2.22044604925031E-16));
#7229=DIRECTION('',(1.,0.,0.));
#7230=DIRECTION('',(0.,-1.,2.22044604925031E-16));
#7231=DIRECTION('',(1.,0.,0.));
#7232=DIRECTION('',(0.,-1.,2.22044604925031E-16));
#7233=DIRECTION('',(1.,0.,0.));
#7234=DIRECTION('',(0.,0.,1.));
#7235=DIRECTION('',(2.22044604925031E-16,1.,0.));
#7236=DIRECTION('',(0.,0.,1.));
#7237=DIRECTION('',(2.22044604925031E-16,-1.,0.));
#7238=DIRECTION('',(0.,0.,1.));
#7239=DIRECTION('',(2.22044604925031E-16,-1.,0.));
#7240=DIRECTION('',(0.,0.,1.));
#7241=DIRECTION('',(2.22044604925031E-16,-1.,0.));
#7242=DIRECTION('',(0.,-1.,2.22044604925031E-16));
#7243=DIRECTION('',(1.,0.,0.));
#7244=DIRECTION('axis',(0.,0.,1.));
#7245=DIRECTION('refdir',(1.,0.,0.));
#7246=DIRECTION('center_axis',(0.,0.,1.));
#7247=DIRECTION('ref_axis',(1.,0.,0.));
#7248=DIRECTION('center_axis',(0.,0.,-1.));
#7249=DIRECTION('ref_axis',(1.,0.,0.));
#7250=DIRECTION('',(0.,0.,-1.));
#7251=DIRECTION('center_axis',(0.,0.,-1.));
#7252=DIRECTION('ref_axis',(1.,0.,0.));
#7253=DIRECTION('center_axis',(0.,0.,1.));
#7254=DIRECTION('ref_axis',(1.,0.,0.));
#7255=DIRECTION('center_axis',(0.,0.,1.));
#7256=DIRECTION('ref_axis',(1.,0.,0.));
#7257=DIRECTION('',(0.,0.,-1.));
#7258=DIRECTION('center_axis',(0.,0.,1.));
#7259=DIRECTION('ref_axis',(1.,0.,0.));
#7260=DIRECTION('center_axis',(0.,0.,1.));
#7261=DIRECTION('ref_axis',(1.,0.,0.));
#7262=DIRECTION('center_axis',(0.,0.,1.));
#7263=DIRECTION('ref_axis',(1.,0.,0.));
#7264=DIRECTION('axis',(0.,0.,1.));
#7265=DIRECTION('refdir',(1.,0.,0.));
#7266=DIRECTION('center_axis',(0.,1.,0.));
#7267=DIRECTION('ref_axis',(1.,0.,0.));
#7268=DIRECTION('center_axis',(0.,-1.,0.));
#7269=DIRECTION('ref_axis',(1.,0.,0.));
#7270=DIRECTION('',(0.,-1.,0.));
#7271=DIRECTION('center_axis',(0.,-1.,0.));
#7272=DIRECTION('ref_axis',(1.,0.,0.));
#7273=DIRECTION('center_axis',(0.,1.,0.));
#7274=DIRECTION('ref_axis',(1.,0.,0.));
#7275=DIRECTION('center_axis',(0.,1.,0.));
#7276=DIRECTION('ref_axis',(1.,0.,0.));
#7277=DIRECTION('',(0.,-1.,0.));
#7278=DIRECTION('center_axis',(0.,1.,0.));
#7279=DIRECTION('ref_axis',(1.,0.,0.));
#7280=DIRECTION('center_axis',(0.,1.,0.));
#7281=DIRECTION('ref_axis',(1.,0.,0.));
#7282=DIRECTION('center_axis',(0.,1.,0.));
#7283=DIRECTION('ref_axis',(1.,0.,0.));
#7284=DIRECTION('axis',(0.,0.,1.));
#7285=DIRECTION('refdir',(1.,0.,0.));
#7286=DIRECTION('center_axis',(0.,1.,0.));
#7287=DIRECTION('ref_axis',(0.,0.,1.));
#7288=DIRECTION('center_axis',(0.,-1.,0.));
#7289=DIRECTION('ref_axis',(1.,0.,0.));
#7290=DIRECTION('center_axis',(0.,-1.,0.));
#7291=DIRECTION('ref_axis',(1.,0.,0.));
#7292=DIRECTION('center_axis',(0.,-1.,0.));
#7293=DIRECTION('ref_axis',(1.,0.,0.));
#7294=DIRECTION('',(0.707106781186548,0.707106781186547,8.65956056235494E-17));
#7295=DIRECTION('center_axis',(0.,-1.,0.));
#7296=DIRECTION('ref_axis',(1.,0.,0.));
#7297=DIRECTION('center_axis',(0.,-1.,0.));
#7298=DIRECTION('ref_axis',(1.,0.,0.));
#7299=DIRECTION('',(0.,1.,0.));
#7300=DIRECTION('center_axis',(0.,1.,0.));
#7301=DIRECTION('ref_axis',(1.,0.,0.));
#7302=DIRECTION('center_axis',(0.,-1.,0.));
#7303=DIRECTION('ref_axis',(1.,0.,0.));
#7304=DIRECTION('',(-0.707106781186547,0.707106781186548,-8.65956056235493E-17));
#7305=DIRECTION('center_axis',(0.,-1.,0.));
#7306=DIRECTION('ref_axis',(0.,0.,-1.));
#7307=DIRECTION('center_axis',(0.,-1.,0.));
#7308=DIRECTION('ref_axis',(1.,0.,0.));
#7309=DIRECTION('center_axis',(0.,1.,0.));
#7310=DIRECTION('ref_axis',(1.,0.,0.));
#7311=DIRECTION('center_axis',(0.,1.,0.));
#7312=DIRECTION('ref_axis',(1.,0.,0.));
#7313=DIRECTION('',(-0.447213595499958,0.894427190999916,-5.47678698264203E-17));
#7314=DIRECTION('center_axis',(0.,-1.,0.));
#7315=DIRECTION('ref_axis',(1.,0.,0.));
#7316=DIRECTION('center_axis',(0.,1.,0.));
#7317=DIRECTION('ref_axis',(1.,0.,0.));
#7318=DIRECTION('',(0.,1.,0.));
#7319=DIRECTION('center_axis',(0.,1.,0.));
#7320=DIRECTION('ref_axis',(1.,0.,0.));
#7321=DIRECTION('center_axis',(0.,-1.,0.));
#7322=DIRECTION('ref_axis',(1.,0.,0.));
#7323=DIRECTION('',(-0.707106781186547,0.707106781186548,-8.65956056235493E-17));
#7324=DIRECTION('center_axis',(0.,-1.,0.));
#7325=DIRECTION('ref_axis',(0.,0.,-1.));
#7326=DIRECTION('center_axis',(0.866025403784439,0.,-0.5));
#7327=DIRECTION('ref_axis',(0.5,0.,0.866025403784439));
#7328=DIRECTION('',(-0.5,0.,-0.866025403784439));
#7329=DIRECTION('',(0.,-1.,0.));
#7330=DIRECTION('',(0.5,0.,0.866025403784439));
#7331=DIRECTION('',(0.,-1.,0.));
#7332=DIRECTION('center_axis',(1.92296268638356E-16,0.,-1.));
#7333=DIRECTION('ref_axis',(1.,0.,1.92296268638356E-16));
#7334=DIRECTION('',(-1.,0.,-1.92296268638356E-16));
#7335=DIRECTION('',(0.,-1.,0.));
#7336=DIRECTION('',(1.,0.,1.92296268638356E-16));
#7337=DIRECTION('center_axis',(-0.866025403784439,0.,-0.5));
#7338=DIRECTION('ref_axis',(0.5,0.,-0.866025403784439));
#7339=DIRECTION('',(-0.5,0.,0.866025403784438));
#7340=DIRECTION('',(0.,-1.,0.));
#7341=DIRECTION('',(0.5,0.,-0.866025403784438));
#7342=DIRECTION('center_axis',(-0.866025403784439,0.,0.5));
#7343=DIRECTION('ref_axis',(-0.5,0.,-0.866025403784439));
#7344=DIRECTION('',(0.5,0.,0.866025403784439));
#7345=DIRECTION('',(0.,-1.,0.));
#7346=DIRECTION('',(-0.5,0.,-0.866025403784439));
#7347=DIRECTION('center_axis',(-1.92296268638356E-16,0.,1.));
#7348=DIRECTION('ref_axis',(-1.,0.,-1.92296268638356E-16));
#7349=DIRECTION('',(1.,0.,1.92296268638356E-16));
#7350=DIRECTION('',(0.,-1.,0.));
#7351=DIRECTION('',(-1.,0.,-1.92296268638356E-16));
#7352=DIRECTION('center_axis',(0.866025403784439,0.,0.5));
#7353=DIRECTION('ref_axis',(-0.5,0.,0.866025403784439));
#7354=DIRECTION('',(0.5,0.,-0.866025403784439));
#7355=DIRECTION('',(-0.5,0.,0.866025403784439));
#7356=DIRECTION('center_axis',(0.,1.,0.));
#7357=DIRECTION('ref_axis',(1.,0.,0.));
#7358=DIRECTION('center_axis',(0.,-1.,0.));
#7359=DIRECTION('ref_axis',(0.,0.,-1.));
#7360=DIRECTION('',(0.,0.,1.));
#7361=DIRECTION('',(1.,0.,0.));
#7362=DIRECTION('',(0.,0.,1.));
#7363=DIRECTION('',(1.,0.,0.));
#7364=DIRECTION('',(0.,0.,1.));
#7365=DIRECTION('',(2.22044604925031E-16,-1.,0.));
#7366=DIRECTION('',(0.,0.,1.));
#7367=DIRECTION('',(2.22044604925031E-16,-1.,0.));
#7368=DIRECTION('',(0.,0.,1.));
#7369=DIRECTION('',(1.,0.,0.));
#7370=DIRECTION('',(0.,0.,1.));
#7371=DIRECTION('',(1.,0.,0.));
#7372=DIRECTION('',(0.,0.,1.));
#7373=DIRECTION('',(2.22044604925031E-16,1.,0.));
#7374=DIRECTION('',(0.,0.,1.));
#7375=DIRECTION('',(2.22044604925031E-16,1.,0.));
#7376=DIRECTION('',(0.,0.,1.));
#7377=DIRECTION('',(2.22044604925031E-16,1.,0.));
#7378=DIRECTION('',(0.,0.,1.));
#7379=DIRECTION('',(2.22044604925031E-16,1.,0.));
#7380=DIRECTION('',(0.,0.,1.));
#7381=DIRECTION('',(2.22044604925031E-16,-1.,0.));
#7382=DIRECTION('',(0.,0.,1.));
#7383=DIRECTION('',(2.22044604925031E-16,-1.,0.));
#7384=DIRECTION('',(0.,0.,1.));
#7385=DIRECTION('',(2.22044604925031E-16,-1.,0.));
#7386=DIRECTION('',(0.,0.,1.));
#7387=DIRECTION('',(2.22044604925031E-16,-1.,0.));
#7388=DIRECTION('',(0.,-1.,2.22044604925031E-16));
#7389=DIRECTION('',(1.,0.,0.));
#7390=DIRECTION('',(0.,-1.,2.22044604925031E-16));
#7391=DIRECTION('',(1.,0.,0.));
#7392=DIRECTION('',(0.,-1.,2.22044604925031E-16));
#7393=DIRECTION('',(1.,0.,0.));
#7394=DIRECTION('',(0.,-1.,2.22044604925031E-16));
#7395=DIRECTION('',(1.,0.,0.));
#7396=DIRECTION('',(0.,0.,1.));
#7397=DIRECTION('',(1.,0.,0.));
#7398=DIRECTION('',(0.,-1.,2.22044604925031E-16));
#7399=DIRECTION('',(1.,0.,0.));
#7400=DIRECTION('',(0.,-1.,2.22044604925031E-16));
#7401=DIRECTION('',(1.,0.,0.));
#7402=DIRECTION('',(0.,0.,1.));
#7403=DIRECTION('',(1.,0.,0.));
#7404=DIRECTION('',(6.12323399573677E-17,-3.74939945665464E-33,1.));
#7405=DIRECTION('',(1.,4.21739888566864E-65,-6.12323399573677E-17));
#7406=CARTESIAN_POINT('',(0.,0.,0.));
#7407=CARTESIAN_POINT('',(0.,0.,0.));
#7408=CARTESIAN_POINT('',(0.,0.,0.));
#7409=CARTESIAN_POINT('Origin',(11.7,-1.6,-0.1));
#7410=CARTESIAN_POINT('',(11.49,-1.6,0.));
#7411=CARTESIAN_POINT('Origin',(11.7,-1.6,0.));
#7412=CARTESIAN_POINT('',(11.49,-1.6,1.));
#7413=CARTESIAN_POINT('',(11.49,-1.6,-0.1));
#7414=CARTESIAN_POINT('Origin',(11.7,-1.6,1.));
#7415=CARTESIAN_POINT('Origin',(9.5,1.6,-0.1));
#7416=CARTESIAN_POINT('',(9.29,1.6,0.));
#7417=CARTESIAN_POINT('Origin',(9.5,1.6,0.));
#7418=CARTESIAN_POINT('',(9.29,1.6,1.));
#7419=CARTESIAN_POINT('',(9.29,1.6,-0.1));
#7420=CARTESIAN_POINT('Origin',(9.5,1.6,1.));
#7421=CARTESIAN_POINT('Origin',(9.5,-1.6,-0.1));
#7422=CARTESIAN_POINT('',(9.29,-1.6,0.));
#7423=CARTESIAN_POINT('Origin',(9.5,-1.6,0.));
#7424=CARTESIAN_POINT('',(9.29,-1.6,1.));
#7425=CARTESIAN_POINT('',(9.29,-1.6,-0.1));
#7426=CARTESIAN_POINT('Origin',(9.5,-1.6,1.));
#7427=CARTESIAN_POINT('Origin',(11.7,1.6,-0.1));
#7428=CARTESIAN_POINT('',(11.49,1.6,0.));
#7429=CARTESIAN_POINT('Origin',(11.7,1.6,0.));
#7430=CARTESIAN_POINT('',(11.49,1.6,1.));
#7431=CARTESIAN_POINT('',(11.49,1.6,-0.1));
#7432=CARTESIAN_POINT('Origin',(11.7,1.6,1.));
#7433=CARTESIAN_POINT('Origin',(26.5,-5.5,-0.1));
#7434=CARTESIAN_POINT('',(26.29,-5.5,0.));
#7435=CARTESIAN_POINT('Origin',(26.5,-5.5,0.));
#7436=CARTESIAN_POINT('',(26.29,-5.5,1.));
#7437=CARTESIAN_POINT('',(26.29,-5.5,-0.1));
#7438=CARTESIAN_POINT('Origin',(26.5,-5.5,1.));
#7439=CARTESIAN_POINT('Origin',(3.5,5.5,-0.1));
#7440=CARTESIAN_POINT('',(3.29,5.5,0.));
#7441=CARTESIAN_POINT('Origin',(3.5,5.5,0.));
#7442=CARTESIAN_POINT('',(3.29,5.5,1.));
#7443=CARTESIAN_POINT('',(3.29,5.5,-0.1));
#7444=CARTESIAN_POINT('Origin',(3.5,5.5,1.));
#7445=CARTESIAN_POINT('Origin',(3.5,-5.5,-0.1));
#7446=CARTESIAN_POINT('',(3.29,-5.5,0.));
#7447=CARTESIAN_POINT('Origin',(3.5,-5.5,0.));
#7448=CARTESIAN_POINT('',(3.29,-5.5,1.));
#7449=CARTESIAN_POINT('',(3.29,-5.5,-0.1));
#7450=CARTESIAN_POINT('Origin',(3.5,-5.5,1.));
#7451=CARTESIAN_POINT('Origin',(26.5,5.5,-0.1));
#7452=CARTESIAN_POINT('',(26.29,5.5,0.));
#7453=CARTESIAN_POINT('Origin',(26.5,5.5,0.));
#7454=CARTESIAN_POINT('',(26.29,5.5,1.));
#7455=CARTESIAN_POINT('',(26.29,5.5,-0.1));
#7456=CARTESIAN_POINT('Origin',(26.5,5.5,1.));
#7457=CARTESIAN_POINT('Origin',(29.,2.4,-0.1));
#7458=CARTESIAN_POINT('',(28.79,2.4,0.));
#7459=CARTESIAN_POINT('Origin',(29.,2.4,0.));
#7460=CARTESIAN_POINT('',(28.79,2.4,1.));
#7461=CARTESIAN_POINT('',(28.79,2.4,-0.1));
#7462=CARTESIAN_POINT('Origin',(29.,2.4,1.));
#7463=CARTESIAN_POINT('Origin',(29.,-5.6,-0.1));
#7464=CARTESIAN_POINT('',(28.79,-5.6,0.));
#7465=CARTESIAN_POINT('Origin',(29.,-5.6,0.));
#7466=CARTESIAN_POINT('',(28.79,-5.6,1.));
#7467=CARTESIAN_POINT('',(28.79,-5.6,-0.1));
#7468=CARTESIAN_POINT('Origin',(29.,-5.6,1.));
#7469=CARTESIAN_POINT('Origin',(1.,5.6,-0.1));
#7470=CARTESIAN_POINT('',(0.79,5.6,0.));
#7471=CARTESIAN_POINT('Origin',(1.,5.6,0.));
#7472=CARTESIAN_POINT('',(0.79,5.6,1.));
#7473=CARTESIAN_POINT('',(0.79,5.6,-0.1));
#7474=CARTESIAN_POINT('Origin',(1.,5.6,1.));
#7475=CARTESIAN_POINT('Origin',(1.,-2.4,-0.1));
#7476=CARTESIAN_POINT('',(0.79,-2.4,0.));
#7477=CARTESIAN_POINT('Origin',(1.,-2.4,0.));
#7478=CARTESIAN_POINT('',(0.79,-2.4,1.));
#7479=CARTESIAN_POINT('',(0.79,-2.4,-0.1));
#7480=CARTESIAN_POINT('Origin',(1.,-2.4,1.));
#7481=CARTESIAN_POINT('Origin',(1.,2.4,-0.1));
#7482=CARTESIAN_POINT('',(0.79,2.4,0.));
#7483=CARTESIAN_POINT('Origin',(1.,2.4,0.));
#7484=CARTESIAN_POINT('',(0.79,2.4,1.));
#7485=CARTESIAN_POINT('',(0.79,2.4,-0.1));
#7486=CARTESIAN_POINT('Origin',(1.,2.4,1.));
#7487=CARTESIAN_POINT('Origin',(1.,-5.6,-0.1));
#7488=CARTESIAN_POINT('',(0.79,-5.6,0.));
#7489=CARTESIAN_POINT('Origin',(1.,-5.6,0.));
#7490=CARTESIAN_POINT('',(0.79,-5.6,1.));
#7491=CARTESIAN_POINT('',(0.79,-5.6,-0.1));
#7492=CARTESIAN_POINT('Origin',(1.,-5.6,1.));
#7493=CARTESIAN_POINT('Origin',(29.,-2.4,-0.1));
#7494=CARTESIAN_POINT('',(28.79,-2.4,0.));
#7495=CARTESIAN_POINT('Origin',(29.,-2.4,0.));
#7496=CARTESIAN_POINT('',(28.79,-2.4,1.));
#7497=CARTESIAN_POINT('',(28.79,-2.4,-0.1));
#7498=CARTESIAN_POINT('Origin',(29.,-2.4,1.));
#7499=CARTESIAN_POINT('Origin',(29.,5.6,-0.1));
#7500=CARTESIAN_POINT('',(28.79,5.6,0.));
#7501=CARTESIAN_POINT('Origin',(29.,5.6,0.));
#7502=CARTESIAN_POINT('',(28.79,5.6,1.));
#7503=CARTESIAN_POINT('',(28.79,5.6,-0.1));
#7504=CARTESIAN_POINT('Origin',(29.,5.6,1.));
#7505=CARTESIAN_POINT('Origin',(31.,7.5,0.));
#7506=CARTESIAN_POINT('',(31.,7.5,0.));
#7507=CARTESIAN_POINT('',(-1.,7.5,0.));
#7508=CARTESIAN_POINT('',(31.,7.5,0.));
#7509=CARTESIAN_POINT('',(-1.,7.5,1.));
#7510=CARTESIAN_POINT('',(-1.,7.5,0.));
#7511=CARTESIAN_POINT('',(31.,7.5,1.));
#7512=CARTESIAN_POINT('',(31.,7.5,1.));
#7513=CARTESIAN_POINT('',(31.,7.5,0.));
#7514=CARTESIAN_POINT('Origin',(31.,-7.5,0.));
#7515=CARTESIAN_POINT('',(31.,-7.5,0.));
#7516=CARTESIAN_POINT('',(31.,-7.5,0.));
#7517=CARTESIAN_POINT('',(31.,-7.5,1.));
#7518=CARTESIAN_POINT('',(31.,-7.5,1.));
#7519=CARTESIAN_POINT('',(31.,-7.5,0.));
#7520=CARTESIAN_POINT('Origin',(-1.,-7.5,0.));
#7521=CARTESIAN_POINT('',(-1.,-7.5,0.));
#7522=CARTESIAN_POINT('',(-1.,-7.5,0.));
#7523=CARTESIAN_POINT('',(-1.,-7.5,1.));
#7524=CARTESIAN_POINT('',(-1.,-7.5,1.));
#7525=CARTESIAN_POINT('',(-1.,-7.5,0.));
#7526=CARTESIAN_POINT('Origin',(-1.,7.5,0.));
#7527=CARTESIAN_POINT('',(-1.,7.5,0.));
#7528=CARTESIAN_POINT('',(-1.,7.5,1.));
#7529=CARTESIAN_POINT('Origin',(15.,0.,1.));
#7530=CARTESIAN_POINT('Origin',(15.,0.,0.));
#7531=CARTESIAN_POINT('',(0.,0.,0.));
#7532=CARTESIAN_POINT('Origin',(0.05,0.,0.));
#7533=CARTESIAN_POINT('',(0.1,7.34788079488412E-17,0.6));
#7534=CARTESIAN_POINT('Origin',(0.1,0.,0.));
#7535=CARTESIAN_POINT('',(0.,-6.12323399573677E-17,0.5));
#7536=CARTESIAN_POINT('',(0.05,-6.73555739531044E-17,0.55));
#7537=CARTESIAN_POINT('Origin',(0.,0.,0.));
#7538=CARTESIAN_POINT('Origin',(0.,0.,0.));
#7539=CARTESIAN_POINT('',(29.9,-7.34788079488412E-17,0.6));
#7540=CARTESIAN_POINT('Origin',(29.9,0.,0.));
#7541=CARTESIAN_POINT('',(0.,-7.34788079488412E-17,0.6));
#7542=CARTESIAN_POINT('Origin',(0.,0.,0.));
#7543=CARTESIAN_POINT('Origin',(29.95,0.,0.));
#7544=CARTESIAN_POINT('',(30.,6.12323399573677E-17,0.5));
#7545=CARTESIAN_POINT('Origin',(30.,0.,0.));
#7546=CARTESIAN_POINT('',(29.95,-6.73555739531044E-17,0.55));
#7547=CARTESIAN_POINT('Origin',(30.,0.,0.));
#7548=CARTESIAN_POINT('',(0.,0.,0.));
#7549=CARTESIAN_POINT('Origin',(-1.6,0.,1.3));
#7550=CARTESIAN_POINT('',(-1.2,0.340036762718386,1.3));
#7551=CARTESIAN_POINT('',(-1.2,-0.340036762718386,1.3));
#7552=CARTESIAN_POINT('',(-1.2,0.,1.3));
#7553=CARTESIAN_POINT('Origin',(-1.6,0.,1.3));
#7554=CARTESIAN_POINT('Origin',(-1.6,0.,0.6));
#7555=CARTESIAN_POINT('',(-1.2,0.340036762718386,0.6));
#7556=CARTESIAN_POINT('',(-1.2,0.340036762718386,0.6));
#7557=CARTESIAN_POINT('',(-1.2,-0.340036762718386,0.6));
#7558=CARTESIAN_POINT('Origin',(-1.6,0.,0.6));
#7559=CARTESIAN_POINT('',(-1.2,-0.340036762718386,0.6));
#7560=CARTESIAN_POINT('Origin',(1.6,0.,0.6));
#7561=CARTESIAN_POINT('',(1.2,0.340036762718386,1.3));
#7562=CARTESIAN_POINT('',(1.2,0.340036762718386,0.6));
#7563=CARTESIAN_POINT('',(1.2,0.340036762718386,0.6));
#7564=CARTESIAN_POINT('',(1.2,-0.340036762718386,1.3));
#7565=CARTESIAN_POINT('Origin',(1.6,0.,1.3));
#7566=CARTESIAN_POINT('',(1.2,-0.340036762718386,0.6));
#7567=CARTESIAN_POINT('',(1.2,-0.340036762718386,0.6));
#7568=CARTESIAN_POINT('Origin',(1.6,0.,0.6));
#7569=CARTESIAN_POINT('Origin',(1.6,0.,1.3));
#7570=CARTESIAN_POINT('',(1.2,0.,1.3));
#7571=CARTESIAN_POINT('Origin',(-2.1,0.,0.6));
#7572=CARTESIAN_POINT('',(-1.2,0.7,0.6));
#7573=CARTESIAN_POINT('',(-1.2,0.,0.6));
#7574=CARTESIAN_POINT('',(-2.1,0.7,0.6));
#7575=CARTESIAN_POINT('',(-1.2,0.7,0.6));
#7576=CARTESIAN_POINT('',(-2.1,-0.7,0.6));
#7577=CARTESIAN_POINT('',(-2.1,0.,0.6));
#7578=CARTESIAN_POINT('',(-1.2,-0.7,0.6));
#7579=CARTESIAN_POINT('',(-1.2,-0.7,0.6));
#7580=CARTESIAN_POINT('',(-1.2,0.,0.6));
#7581=CARTESIAN_POINT('',(-1.875,3.36777869765522E-17,0.6));
#7582=CARTESIAN_POINT('Origin',(-1.6,0.,0.6));
#7583=CARTESIAN_POINT('Origin',(-1.2,0.,0.6));
#7584=CARTESIAN_POINT('',(-1.2,-0.7,3.75));
#7585=CARTESIAN_POINT('',(-1.2,-0.7,3.75));
#7586=CARTESIAN_POINT('',(-1.2,0.7,3.75));
#7587=CARTESIAN_POINT('',(-1.2,0.,3.75));
#7588=CARTESIAN_POINT('',(-1.2,0.7,3.75));
#7589=CARTESIAN_POINT('',(-1.2,-2.02066721859313E-17,3.515));
#7590=CARTESIAN_POINT('Origin',(-1.2,0.,3.35));
#7591=CARTESIAN_POINT('Origin',(1.2,0.,0.6));
#7592=CARTESIAN_POINT('',(2.1,-0.7,0.6));
#7593=CARTESIAN_POINT('',(2.1,0.7,0.6));
#7594=CARTESIAN_POINT('',(2.1,0.,0.6));
#7595=CARTESIAN_POINT('',(1.2,0.7,0.6));
#7596=CARTESIAN_POINT('',(2.1,0.7,0.6));
#7597=CARTESIAN_POINT('',(1.2,0.,0.6));
#7598=CARTESIAN_POINT('',(1.2,-0.7,0.6));
#7599=CARTESIAN_POINT('',(1.2,0.,0.6));
#7600=CARTESIAN_POINT('',(2.1,-0.7,0.6));
#7601=CARTESIAN_POINT('',(1.325,3.36777869765522E-17,0.6));
#7602=CARTESIAN_POINT('Origin',(1.6,0.,0.6));
#7603=CARTESIAN_POINT('Origin',(0.1,0.,3.35));
#7604=CARTESIAN_POINT('',(0.1,-2.75545529808155E-17,3.575));
#7605=CARTESIAN_POINT('Origin',(0.1,0.,3.35));
#7606=CARTESIAN_POINT('',(1.2,2.75545529808155E-17,3.575));
#7607=CARTESIAN_POINT('',(0.1,-2.75545529808155E-17,3.575));
#7608=CARTESIAN_POINT('Origin',(1.2,0.,3.35));
#7609=CARTESIAN_POINT('Origin',(0.,0.,3.35));
#7610=CARTESIAN_POINT('',(-0.1,2.02066721859313E-17,3.515));
#7611=CARTESIAN_POINT('',(0.,-2.02066721859313E-17,3.515));
#7612=CARTESIAN_POINT('Origin',(-0.1,0.,3.35));
#7613=CARTESIAN_POINT('Origin',(-1.6,0.,-0.05));
#7614=CARTESIAN_POINT('',(-1.875,-3.36777869765522E-17,0.));
#7615=CARTESIAN_POINT('Origin',(-1.6,0.,0.));
#7616=CARTESIAN_POINT('',(-1.875,-3.36777869765522E-17,-0.05));
#7617=CARTESIAN_POINT('Origin',(1.6,0.,-0.05));
#7618=CARTESIAN_POINT('',(1.325,-3.36777869765522E-17,0.));
#7619=CARTESIAN_POINT('Origin',(1.6,0.,0.));
#7620=CARTESIAN_POINT('',(1.325,-3.36777869765522E-17,-0.05));
#7621=CARTESIAN_POINT('Origin',(0.,0.,2.3));
#7622=CARTESIAN_POINT('',(-0.6,-0.7,2.3));
#7623=CARTESIAN_POINT('Origin',(0.,-0.7,2.3));
#7624=CARTESIAN_POINT('',(-0.6,0.7,2.3));
#7625=CARTESIAN_POINT('',(-0.6,0.,2.3));
#7626=CARTESIAN_POINT('Origin',(0.,0.7,2.3));
#7627=CARTESIAN_POINT('Origin',(0.,-0.7,1.875));
#7628=CARTESIAN_POINT('',(-2.1,-0.7,0.));
#7629=CARTESIAN_POINT('',(-2.1,-0.7,0.6));
#7630=CARTESIAN_POINT('',(2.1,-0.7,0.));
#7631=CARTESIAN_POINT('',(-2.1,-0.7,0.));
#7632=CARTESIAN_POINT('',(2.1,-0.7,0.));
#7633=CARTESIAN_POINT('',(1.2,-0.7,3.75));
#7634=CARTESIAN_POINT('',(1.2,-0.7,0.6));
#7635=CARTESIAN_POINT('',(0.1,-0.7,3.75));
#7636=CARTESIAN_POINT('',(1.2,-0.7,3.75));
#7637=CARTESIAN_POINT('',(0.1,-0.7,2.95));
#7638=CARTESIAN_POINT('',(0.1,-0.7,3.75));
#7639=CARTESIAN_POINT('',(-0.1,-0.7,2.95));
#7640=CARTESIAN_POINT('',(0.1,-0.7,2.95));
#7641=CARTESIAN_POINT('',(-0.1,-0.7,3.75));
#7642=CARTESIAN_POINT('',(-0.1,-0.7,2.95));
#7643=CARTESIAN_POINT('',(-0.1,-0.7,3.75));
#7644=CARTESIAN_POINT('Origin',(-2.1,0.,0.));
#7645=CARTESIAN_POINT('',(-2.1,0.7,0.));
#7646=CARTESIAN_POINT('',(-2.1,0.7,0.6));
#7647=CARTESIAN_POINT('',(-2.1,0.,0.));
#7648=CARTESIAN_POINT('Origin',(2.1,0.,0.));
#7649=CARTESIAN_POINT('',(2.1,0.7,0.));
#7650=CARTESIAN_POINT('',(-2.1,0.7,0.));
#7651=CARTESIAN_POINT('',(2.1,0.,0.));
#7652=CARTESIAN_POINT('Origin',(2.1,0.,0.6));
#7653=CARTESIAN_POINT('',(2.1,0.7,0.));
#7654=CARTESIAN_POINT('Origin',(1.2,0.,3.75));
#7655=CARTESIAN_POINT('',(1.2,0.7,3.75));
#7656=CARTESIAN_POINT('',(1.2,0.7,0.6));
#7657=CARTESIAN_POINT('',(1.2,0.,3.75));
#7658=CARTESIAN_POINT('Origin',(0.1,0.,3.75));
#7659=CARTESIAN_POINT('',(0.1,0.7,3.75));
#7660=CARTESIAN_POINT('',(1.2,0.7,3.75));
#7661=CARTESIAN_POINT('',(0.1,0.,3.75));
#7662=CARTESIAN_POINT('Origin',(0.1,0.,2.95));
#7663=CARTESIAN_POINT('',(0.1,0.7,2.95));
#7664=CARTESIAN_POINT('',(0.1,0.7,3.75));
#7665=CARTESIAN_POINT('',(0.1,0.,2.95));
#7666=CARTESIAN_POINT('Origin',(-0.1,0.,2.95));
#7667=CARTESIAN_POINT('',(-0.1,0.7,2.95));
#7668=CARTESIAN_POINT('',(0.1,0.7,2.95));
#7669=CARTESIAN_POINT('',(-0.1,0.,2.95));
#7670=CARTESIAN_POINT('Origin',(-0.1,0.,3.75));
#7671=CARTESIAN_POINT('',(-0.1,0.7,3.75));
#7672=CARTESIAN_POINT('',(-0.1,0.7,2.95));
#7673=CARTESIAN_POINT('',(-0.1,0.,3.75));
#7674=CARTESIAN_POINT('Origin',(-1.2,0.,3.75));
#7675=CARTESIAN_POINT('',(-0.1,0.7,3.75));
#7676=CARTESIAN_POINT('Origin',(0.,0.7,1.875));
#7677=CARTESIAN_POINT('',(0.,0.,0.));
#7678=CARTESIAN_POINT('Origin',(0.115470053837925,-0.5,-0.2));
#7679=CARTESIAN_POINT('',(0.23094010767585,-0.5,0.));
#7680=CARTESIAN_POINT('',(0.115470053837925,-0.5,-0.2));
#7681=CARTESIAN_POINT('',(0.23094010767585,-0.5,0.));
#7682=CARTESIAN_POINT('',(0.115470053837925,-0.8,-0.2));
#7683=CARTESIAN_POINT('',(0.115470053837925,-0.5,-0.2));
#7684=CARTESIAN_POINT('',(0.23094010767585,-0.8,0.));
#7685=CARTESIAN_POINT('',(0.23094010767585,-0.8,0.));
#7686=CARTESIAN_POINT('',(0.23094010767585,-0.5,0.));
#7687=CARTESIAN_POINT('Origin',(-0.115470053837925,-0.5,-0.2));
#7688=CARTESIAN_POINT('',(-0.115470053837925,-0.5,-0.2));
#7689=CARTESIAN_POINT('',(0.115470053837925,-0.5,-0.2));
#7690=CARTESIAN_POINT('',(-0.115470053837925,-0.8,-0.2));
#7691=CARTESIAN_POINT('',(-0.115470053837925,-0.5,-0.2));
#7692=CARTESIAN_POINT('',(0.115470053837925,-0.8,-0.2));
#7693=CARTESIAN_POINT('Origin',(-0.23094010767585,-0.5,-2.77555756156289E-17));
#7694=CARTESIAN_POINT('',(-0.23094010767585,-0.5,-2.82820063659975E-17));
#7695=CARTESIAN_POINT('',(-0.115470053837925,-0.5,-0.2));
#7696=CARTESIAN_POINT('',(-0.23094010767585,-0.8,-2.77555756156289E-17));
#7697=CARTESIAN_POINT('',(-0.23094010767585,-0.5,-2.82820063659975E-17));
#7698=CARTESIAN_POINT('',(-0.115470053837925,-0.8,-0.2));
#7699=CARTESIAN_POINT('Origin',(-0.115470053837925,-0.5,0.2));
#7700=CARTESIAN_POINT('',(-0.115470053837925,-0.5,0.2));
#7701=CARTESIAN_POINT('',(-0.23094010767585,-0.5,-2.82820063659975E-17));
#7702=CARTESIAN_POINT('',(-0.115470053837925,-0.8,0.2));
#7703=CARTESIAN_POINT('',(-0.115470053837925,-0.5,0.2));
#7704=CARTESIAN_POINT('',(-0.23094010767585,-0.8,-2.82820063659975E-17));
#7705=CARTESIAN_POINT('Origin',(0.115470053837925,-0.5,0.2));
#7706=CARTESIAN_POINT('',(0.115470053837925,-0.5,0.2));
#7707=CARTESIAN_POINT('',(-0.115470053837925,-0.5,0.2));
#7708=CARTESIAN_POINT('',(0.115470053837925,-0.8,0.2));
#7709=CARTESIAN_POINT('',(0.115470053837925,-0.5,0.2));
#7710=CARTESIAN_POINT('',(-0.115470053837925,-0.8,0.2));
#7711=CARTESIAN_POINT('Origin',(0.23094010767585,-0.5,0.));
#7712=CARTESIAN_POINT('',(0.115470053837925,-0.5,0.2));
#7713=CARTESIAN_POINT('',(0.115470053837925,-0.8,0.2));
#7714=CARTESIAN_POINT('Origin',(0.,-0.5,0.));
#7715=CARTESIAN_POINT('Origin',(0.,-0.8,0.));
#7716=CARTESIAN_POINT('Origin',(0.,-1.4,0.));
#7717=CARTESIAN_POINT('',(-0.24505,-1.4,3.00099698131059E-17));
#7718=CARTESIAN_POINT('Origin',(0.,-1.4,0.));
#7719=CARTESIAN_POINT('Origin',(0.375,0.5,0.));
#7720=CARTESIAN_POINT('',(-0.375,0.5,-4.59242549680257E-17));
#7721=CARTESIAN_POINT('Origin',(0.,0.5,0.));
#7722=CARTESIAN_POINT('Origin',(0.,0.475,0.));
#7723=CARTESIAN_POINT('',(-0.425,0.45,-5.20474889637625E-17));
#7724=CARTESIAN_POINT('Origin',(0.,0.45,0.));
#7725=CARTESIAN_POINT('',(-0.4,0.475,-4.89858719658941E-17));
#7726=CARTESIAN_POINT('Origin',(0.,0.24,0.));
#7727=CARTESIAN_POINT('',(-0.425,0.0299999999999998,-5.20474889637625E-17));
#7728=CARTESIAN_POINT('Origin',(0.,0.0299999999999998,0.));
#7729=CARTESIAN_POINT('',(-0.425,0.24,-5.20474889637625E-17));
#7730=CARTESIAN_POINT('Origin',(0.,0.0150000000000001,0.));
#7731=CARTESIAN_POINT('',(-0.395,4.85722573273506E-17,-4.83735485663204E-17));
#7732=CARTESIAN_POINT('Origin',(0.,0.,0.));
#7733=CARTESIAN_POINT('',(-0.41,0.0150000000000001,-5.02105187650415E-17));
#7734=CARTESIAN_POINT('Origin',(0.27,0.,0.));
#7735=CARTESIAN_POINT('',(-0.27,0.,-3.30654635769785E-17));
#7736=CARTESIAN_POINT('Origin',(0.,0.,0.));
#7737=CARTESIAN_POINT('Origin',(0.,-0.02,0.));
#7738=CARTESIAN_POINT('',(-0.24505,-0.0498999999999999,3.00099698131059E-17));
#7739=CARTESIAN_POINT('Origin',(0.,-0.0498999999999999,0.));
#7740=CARTESIAN_POINT('',(-0.26,-0.02,-3.18408167778312E-17));
#7741=CARTESIAN_POINT('Origin',(0.,-0.995,0.));
#7742=CARTESIAN_POINT('',(-0.24505,-0.995,-3.00099698131059E-17));
#7743=CARTESIAN_POINT('',(0.,0.,0.));
#7744=CARTESIAN_POINT('Origin',(3.5,-5.5,2.));
#7745=CARTESIAN_POINT('',(3.025,-5.5,2.));
#7746=CARTESIAN_POINT('Origin',(3.5,-5.5,2.));
#7747=CARTESIAN_POINT('',(3.025,-5.5,2.5));
#7748=CARTESIAN_POINT('',(3.025,-5.5,2.));
#7749=CARTESIAN_POINT('Origin',(3.5,-5.5,2.5));
#7750=CARTESIAN_POINT('Origin',(3.5,-5.5,2.));
#7751=CARTESIAN_POINT('',(3.225,-5.5,2.));
#7752=CARTESIAN_POINT('Origin',(3.5,-5.5,2.));
#7753=CARTESIAN_POINT('Origin',(3.5,5.5,2.));
#7754=CARTESIAN_POINT('',(3.025,5.5,2.));
#7755=CARTESIAN_POINT('Origin',(3.5,5.5,2.));
#7756=CARTESIAN_POINT('',(3.025,5.5,2.5));
#7757=CARTESIAN_POINT('',(3.025,5.5,2.));
#7758=CARTESIAN_POINT('Origin',(3.5,5.5,2.5));
#7759=CARTESIAN_POINT('Origin',(3.5,5.5,2.));
#7760=CARTESIAN_POINT('',(3.225,5.5,2.));
#7761=CARTESIAN_POINT('Origin',(3.5,5.5,2.));
#7762=CARTESIAN_POINT('Origin',(3.5,-5.5,0.9));
#7763=CARTESIAN_POINT('',(3.225,-5.5,1.));
#7764=CARTESIAN_POINT('Origin',(3.5,-5.5,1.));
#7765=CARTESIAN_POINT('',(3.225,-5.5,0.9));
#7766=CARTESIAN_POINT('Origin',(3.5,5.5,0.9));
#7767=CARTESIAN_POINT('',(3.225,5.5,1.));
#7768=CARTESIAN_POINT('Origin',(3.5,5.5,1.));
#7769=CARTESIAN_POINT('',(3.225,5.5,0.9));
#7770=CARTESIAN_POINT('Origin',(4.,6.5,1.));
#7771=CARTESIAN_POINT('',(4.,6.5,1.));
#7772=CARTESIAN_POINT('',(3.,6.5,1.));
#7773=CARTESIAN_POINT('',(4.,6.5,1.));
#7774=CARTESIAN_POINT('',(3.,6.5,2.5));
#7775=CARTESIAN_POINT('',(3.,6.5,1.));
#7776=CARTESIAN_POINT('',(4.,6.5,2.5));
#7777=CARTESIAN_POINT('',(4.,6.5,2.5));
#7778=CARTESIAN_POINT('',(4.,6.5,1.));
#7779=CARTESIAN_POINT('Origin',(4.,-6.5,1.));
#7780=CARTESIAN_POINT('',(4.,-6.5,1.));
#7781=CARTESIAN_POINT('',(4.,-6.5,1.));
#7782=CARTESIAN_POINT('',(4.,-6.5,2.5));
#7783=CARTESIAN_POINT('',(4.,-6.5,2.5));
#7784=CARTESIAN_POINT('',(4.,-6.5,1.));
#7785=CARTESIAN_POINT('Origin',(3.,-6.5,1.));
#7786=CARTESIAN_POINT('',(3.,-6.5,1.));
#7787=CARTESIAN_POINT('',(3.,-6.5,1.));
#7788=CARTESIAN_POINT('',(3.,-6.5,2.5));
#7789=CARTESIAN_POINT('',(3.,-6.5,2.5));
#7790=CARTESIAN_POINT('',(3.,-6.5,1.));
#7791=CARTESIAN_POINT('Origin',(3.,6.5,1.));
#7792=CARTESIAN_POINT('',(3.,6.5,1.));
#7793=CARTESIAN_POINT('',(3.,6.5,2.5));
#7794=CARTESIAN_POINT('Origin',(3.5,0.,2.5));
#7795=CARTESIAN_POINT('Origin',(3.5,0.,1.));
#7796=CARTESIAN_POINT('',(0.,0.,0.));
#7797=CARTESIAN_POINT('Origin',(4.2,6.,1.6));
#7798=CARTESIAN_POINT('',(4.2,6.,1.6));
#7799=CARTESIAN_POINT('',(4.,6.,1.6));
#7800=CARTESIAN_POINT('',(4.2,6.,1.6));
#7801=CARTESIAN_POINT('',(4.,6.,2.5));
#7802=CARTESIAN_POINT('',(4.,6.,1.6));
#7803=CARTESIAN_POINT('',(4.2,6.,2.5));
#7804=CARTESIAN_POINT('',(4.2,6.,2.5));
#7805=CARTESIAN_POINT('',(4.2,6.,1.6));
#7806=CARTESIAN_POINT('Origin',(4.2,-6.,1.6));
#7807=CARTESIAN_POINT('',(4.2,-6.,1.6));
#7808=CARTESIAN_POINT('',(4.2,-6.,1.6));
#7809=CARTESIAN_POINT('',(4.2,-6.,2.5));
#7810=CARTESIAN_POINT('',(4.2,-6.,2.5));
#7811=CARTESIAN_POINT('',(4.2,-6.,1.6));
#7812=CARTESIAN_POINT('Origin',(4.,-6.,1.6));
#7813=CARTESIAN_POINT('',(4.,-6.,1.6));
#7814=CARTESIAN_POINT('',(4.,-6.,1.6));
#7815=CARTESIAN_POINT('',(4.,-6.,2.5));
#7816=CARTESIAN_POINT('',(4.,-6.,2.5));
#7817=CARTESIAN_POINT('',(4.,-6.,1.6));
#7818=CARTESIAN_POINT('Origin',(4.,6.,1.6));
#7819=CARTESIAN_POINT('',(4.,6.,1.6));
#7820=CARTESIAN_POINT('',(4.,6.,2.5));
#7821=CARTESIAN_POINT('Origin',(4.1,0.,2.5));
#7822=CARTESIAN_POINT('Origin',(4.1,0.,1.6));
#7823=CARTESIAN_POINT('',(0.,0.,0.));
#7824=CARTESIAN_POINT('Origin',(10.1,0.,3.3));
#7825=CARTESIAN_POINT('',(10.2,-4.163799117101E-17,3.64));
#7826=CARTESIAN_POINT('Origin',(10.2,0.,3.3));
#7827=CARTESIAN_POINT('',(11.2,4.163799117101E-17,3.64));
#7828=CARTESIAN_POINT('',(10.1,-4.163799117101E-17,3.64));
#7829=CARTESIAN_POINT('Origin',(11.2,0.,3.3));
#7830=CARTESIAN_POINT('Origin',(11.7,-1.6,0.9));
#7831=CARTESIAN_POINT('',(11.425,-1.6,1.));
#7832=CARTESIAN_POINT('Origin',(11.7,-1.6,1.));
#7833=CARTESIAN_POINT('',(11.425,-1.6,1.8));
#7834=CARTESIAN_POINT('',(11.425,-1.6,0.9));
#7835=CARTESIAN_POINT('Origin',(11.7,-1.6,1.8));
#7836=CARTESIAN_POINT('Origin',(9.5,1.6,0.9));
#7837=CARTESIAN_POINT('',(9.225,1.6,1.));
#7838=CARTESIAN_POINT('Origin',(9.5,1.6,1.));
#7839=CARTESIAN_POINT('',(9.225,1.6,1.8));
#7840=CARTESIAN_POINT('',(9.225,1.6,0.9));
#7841=CARTESIAN_POINT('Origin',(9.5,1.6,1.8));
#7842=CARTESIAN_POINT('Origin',(9.5,-1.6,0.9));
#7843=CARTESIAN_POINT('',(9.225,-1.6,1.));
#7844=CARTESIAN_POINT('Origin',(9.5,-1.6,1.));
#7845=CARTESIAN_POINT('',(9.225,-1.6,1.8));
#7846=CARTESIAN_POINT('',(9.225,-1.6,0.9));
#7847=CARTESIAN_POINT('Origin',(9.5,-1.6,1.8));
#7848=CARTESIAN_POINT('Origin',(11.7,1.6,0.9));
#7849=CARTESIAN_POINT('',(11.425,1.6,1.));
#7850=CARTESIAN_POINT('Origin',(11.7,1.6,1.));
#7851=CARTESIAN_POINT('',(11.425,1.6,1.8));
#7852=CARTESIAN_POINT('',(11.425,1.6,0.9));
#7853=CARTESIAN_POINT('Origin',(11.7,1.6,1.8));
#7854=CARTESIAN_POINT('Origin',(10.2,1.,4.5));
#7855=CARTESIAN_POINT('',(10.2,1.,4.5));
#7856=CARTESIAN_POINT('',(10.2,-1.,4.5));
#7857=CARTESIAN_POINT('',(10.2,1.,4.5));
#7858=CARTESIAN_POINT('',(11.2,-1.,4.5));
#7859=CARTESIAN_POINT('',(10.2,-1.,4.5));
#7860=CARTESIAN_POINT('',(11.2,1.,4.5));
#7861=CARTESIAN_POINT('',(11.2,1.,4.5));
#7862=CARTESIAN_POINT('',(10.2,1.,4.5));
#7863=CARTESIAN_POINT('Origin',(10.2,1.,1.8));
#7864=CARTESIAN_POINT('',(10.2,1.,1.8));
#7865=CARTESIAN_POINT('',(10.2,1.,1.8));
#7866=CARTESIAN_POINT('',(11.2,1.,1.8));
#7867=CARTESIAN_POINT('',(11.2,1.,1.8));
#7868=CARTESIAN_POINT('',(10.35,1.,1.8));
#7869=CARTESIAN_POINT('Origin',(10.2,-1.,4.5));
#7870=CARTESIAN_POINT('',(10.2,-1.,1.8));
#7871=CARTESIAN_POINT('',(10.2,-1.,4.5));
#7872=CARTESIAN_POINT('',(11.2,-1.,1.8));
#7873=CARTESIAN_POINT('',(10.35,-1.,1.8));
#7874=CARTESIAN_POINT('',(11.2,-1.,4.5));
#7875=CARTESIAN_POINT('Origin',(11.2,0.,3.15));
#7876=CARTESIAN_POINT('',(11.2,0.,1.8));
#7877=CARTESIAN_POINT('Origin',(10.2,0.,3.15));
#7878=CARTESIAN_POINT('',(10.2,0.,1.8));
#7879=CARTESIAN_POINT('Origin',(12.,2.,1.));
#7880=CARTESIAN_POINT('',(12.,2.,1.));
#7881=CARTESIAN_POINT('',(9.,2.,1.));
#7882=CARTESIAN_POINT('',(12.,2.,1.));
#7883=CARTESIAN_POINT('',(9.,2.,1.8));
#7884=CARTESIAN_POINT('',(9.,2.,1.));
#7885=CARTESIAN_POINT('',(12.,2.,1.8));
#7886=CARTESIAN_POINT('',(12.,2.,1.8));
#7887=CARTESIAN_POINT('',(12.,2.,1.));
#7888=CARTESIAN_POINT('Origin',(12.,-2.,1.));
#7889=CARTESIAN_POINT('',(12.,-2.,1.));
#7890=CARTESIAN_POINT('',(12.,-2.,1.));
#7891=CARTESIAN_POINT('',(12.,-2.,1.8));
#7892=CARTESIAN_POINT('',(12.,-2.,1.8));
#7893=CARTESIAN_POINT('',(12.,-2.,1.));
#7894=CARTESIAN_POINT('Origin',(9.,-2.,1.));
#7895=CARTESIAN_POINT('',(9.,-2.,1.));
#7896=CARTESIAN_POINT('',(9.,-2.,1.));
#7897=CARTESIAN_POINT('',(9.,-2.,1.8));
#7898=CARTESIAN_POINT('',(9.,-2.,1.8));
#7899=CARTESIAN_POINT('',(9.,-2.,1.));
#7900=CARTESIAN_POINT('Origin',(9.,2.,1.));
#7901=CARTESIAN_POINT('',(9.,2.,1.));
#7902=CARTESIAN_POINT('',(9.,2.,1.8));
#7903=CARTESIAN_POINT('Origin',(10.5,0.,1.8));
#7904=CARTESIAN_POINT('Origin',(10.5,0.,1.));
#7905=CARTESIAN_POINT('',(0.,0.,0.));
#7906=CARTESIAN_POINT('Origin',(0.115470053837925,-0.5,-0.2));
#7907=CARTESIAN_POINT('',(0.23094010767585,-0.5,0.));
#7908=CARTESIAN_POINT('',(0.115470053837925,-0.5,-0.2));
#7909=CARTESIAN_POINT('',(0.23094010767585,-0.5,0.));
#7910=CARTESIAN_POINT('',(0.115470053837925,-0.8,-0.2));
#7911=CARTESIAN_POINT('',(0.115470053837925,-0.5,-0.2));
#7912=CARTESIAN_POINT('',(0.23094010767585,-0.8,0.));
#7913=CARTESIAN_POINT('',(0.23094010767585,-0.8,0.));
#7914=CARTESIAN_POINT('',(0.23094010767585,-0.5,0.));
#7915=CARTESIAN_POINT('Origin',(-0.115470053837925,-0.5,-0.2));
#7916=CARTESIAN_POINT('',(-0.115470053837925,-0.5,-0.2));
#7917=CARTESIAN_POINT('',(0.115470053837925,-0.5,-0.2));
#7918=CARTESIAN_POINT('',(-0.115470053837925,-0.8,-0.2));
#7919=CARTESIAN_POINT('',(-0.115470053837925,-0.5,-0.2));
#7920=CARTESIAN_POINT('',(0.115470053837925,-0.8,-0.2));
#7921=CARTESIAN_POINT('Origin',(-0.23094010767585,-0.5,-2.77555756156289E-17));
#7922=CARTESIAN_POINT('',(-0.23094010767585,-0.5,-2.82820063659975E-17));
#7923=CARTESIAN_POINT('',(-0.115470053837925,-0.5,-0.2));
#7924=CARTESIAN_POINT('',(-0.23094010767585,-0.8,-2.77555756156289E-17));
#7925=CARTESIAN_POINT('',(-0.23094010767585,-0.5,-2.82820063659975E-17));
#7926=CARTESIAN_POINT('',(-0.115470053837925,-0.8,-0.2));
#7927=CARTESIAN_POINT('Origin',(-0.115470053837925,-0.5,0.2));
#7928=CARTESIAN_POINT('',(-0.115470053837925,-0.5,0.2));
#7929=CARTESIAN_POINT('',(-0.23094010767585,-0.5,-2.82820063659975E-17));
#7930=CARTESIAN_POINT('',(-0.115470053837925,-0.8,0.2));
#7931=CARTESIAN_POINT('',(-0.115470053837925,-0.5,0.2));
#7932=CARTESIAN_POINT('',(-0.23094010767585,-0.8,-2.82820063659975E-17));
#7933=CARTESIAN_POINT('Origin',(0.115470053837925,-0.5,0.2));
#7934=CARTESIAN_POINT('',(0.115470053837925,-0.5,0.2));
#7935=CARTESIAN_POINT('',(-0.115470053837925,-0.5,0.2));
#7936=CARTESIAN_POINT('',(0.115470053837925,-0.8,0.2));
#7937=CARTESIAN_POINT('',(0.115470053837925,-0.5,0.2));
#7938=CARTESIAN_POINT('',(-0.115470053837925,-0.8,0.2));
#7939=CARTESIAN_POINT('Origin',(0.23094010767585,-0.5,0.));
#7940=CARTESIAN_POINT('',(0.115470053837925,-0.5,0.2));
#7941=CARTESIAN_POINT('',(0.115470053837925,-0.8,0.2));
#7942=CARTESIAN_POINT('Origin',(0.,-0.5,0.));
#7943=CARTESIAN_POINT('Origin',(0.,-0.8,0.));
#7944=CARTESIAN_POINT('Origin',(0.,-1.4,0.));
#7945=CARTESIAN_POINT('',(-0.24505,-1.4,3.00099698131059E-17));
#7946=CARTESIAN_POINT('Origin',(0.,-1.4,0.));
#7947=CARTESIAN_POINT('Origin',(0.375,0.5,0.));
#7948=CARTESIAN_POINT('',(-0.375,0.5,-4.59242549680257E-17));
#7949=CARTESIAN_POINT('Origin',(0.,0.5,0.));
#7950=CARTESIAN_POINT('Origin',(0.,0.475,0.));
#7951=CARTESIAN_POINT('',(-0.425,0.45,-5.20474889637625E-17));
#7952=CARTESIAN_POINT('Origin',(0.,0.45,0.));
#7953=CARTESIAN_POINT('',(-0.4,0.475,-4.89858719658941E-17));
#7954=CARTESIAN_POINT('Origin',(0.,0.24,0.));
#7955=CARTESIAN_POINT('',(-0.425,0.0299999999999998,-5.20474889637625E-17));
#7956=CARTESIAN_POINT('Origin',(0.,0.0299999999999998,0.));
#7957=CARTESIAN_POINT('',(-0.425,0.24,-5.20474889637625E-17));
#7958=CARTESIAN_POINT('Origin',(0.,0.0150000000000001,0.));
#7959=CARTESIAN_POINT('',(-0.395,4.85722573273506E-17,-4.83735485663204E-17));
#7960=CARTESIAN_POINT('Origin',(0.,0.,0.));
#7961=CARTESIAN_POINT('',(-0.41,0.0150000000000001,-5.02105187650415E-17));
#7962=CARTESIAN_POINT('Origin',(0.27,0.,0.));
#7963=CARTESIAN_POINT('',(-0.27,0.,-3.30654635769785E-17));
#7964=CARTESIAN_POINT('Origin',(0.,0.,0.));
#7965=CARTESIAN_POINT('Origin',(0.,-0.02,0.));
#7966=CARTESIAN_POINT('',(-0.24505,-0.0498999999999999,3.00099698131059E-17));
#7967=CARTESIAN_POINT('Origin',(0.,-0.0498999999999999,0.));
#7968=CARTESIAN_POINT('',(-0.26,-0.02,-3.18408167778312E-17));
#7969=CARTESIAN_POINT('Origin',(0.,-0.995,0.));
#7970=CARTESIAN_POINT('',(-0.24505,-0.995,-3.00099698131059E-17));
#7971=CARTESIAN_POINT('',(0.,0.,0.));
#7972=CARTESIAN_POINT('Origin',(0.,-1.935,0.));
#7973=CARTESIAN_POINT('',(-0.3933,-3.9267,4.81653586104654E-17));
#7974=CARTESIAN_POINT('Origin',(0.,-3.9267,0.));
#7975=CARTESIAN_POINT('',(-0.3933,0.,-4.81653586104654E-17));
#7976=CARTESIAN_POINT('',(-0.3933,-1.935,-4.81653586104654E-17));
#7977=CARTESIAN_POINT('Origin',(0.,0.,0.));
#7978=CARTESIAN_POINT('Origin',(0.,-3.96,0.));
#7979=CARTESIAN_POINT('',(-0.32,-4.,-3.91886975727153E-17));
#7980=CARTESIAN_POINT('Origin',(0.,-4.,0.));
#7981=CARTESIAN_POINT('',(-0.36,-3.96,-4.40872847693047E-17));
#7982=CARTESIAN_POINT('Origin',(0.,-4.,0.));
#7983=CARTESIAN_POINT('Origin',(0.,0.462722715486149,0.));
#7984=CARTESIAN_POINT('',(-0.6175,0.53,-7.5621939847349E-17));
#7985=CARTESIAN_POINT('Origin',(0.,0.53,0.));
#7986=CARTESIAN_POINT('',(-0.750555349946514,0.453180457891261,-9.19165206894919E-17));
#7987=CARTESIAN_POINT('',(-0.734027674973257,0.462722715486149,-8.98924642641573E-17));
#7988=CARTESIAN_POINT('',(-0.375277674973257,0.453180457891261,0.65));
#7989=CARTESIAN_POINT('Ctrl Pts',(-0.375277674973257,0.45318045789126,0.65));
#7990=CARTESIAN_POINT('Ctrl Pts',(-0.562916512459968,0.561513791224244,
0.324999999999856));
#7991=CARTESIAN_POINT('Ctrl Pts',(-0.750555349946514,0.45318045789126,-9.19165206894919E-17));
#7992=CARTESIAN_POINT('',(0.375277674973257,0.453180457891261,0.65));
#7993=CARTESIAN_POINT('Ctrl Pts',(0.375277674973257,0.453180457891261,0.65));
#7994=CARTESIAN_POINT('Ctrl Pts',(-1.66922031752392E-13,0.561513791224244,
0.65));
#7995=CARTESIAN_POINT('Ctrl Pts',(-0.375277674973257,0.45318045789126,0.65));
#7996=CARTESIAN_POINT('',(0.750555349946514,0.453180457891261,0.));
#7997=CARTESIAN_POINT('Ctrl Pts',(0.750555349946514,0.453180457891261,0.));
#7998=CARTESIAN_POINT('Ctrl Pts',(0.562916512459802,0.561513791224244,0.325000000000144));
#7999=CARTESIAN_POINT('Ctrl Pts',(0.375277674973257,0.45318045789126,0.65));
#8000=CARTESIAN_POINT('',(0.375277674973257,0.453180457891261,-0.65));
#8001=CARTESIAN_POINT('Ctrl Pts',(0.375277674973257,0.45318045789126,-0.65));
#8002=CARTESIAN_POINT('Ctrl Pts',(0.562916512459968,0.561513791224244,-0.324999999999855));
#8003=CARTESIAN_POINT('Ctrl Pts',(0.750555349946514,0.453180457891261,0.));
#8004=CARTESIAN_POINT('',(-0.375277674973257,0.45318045789126,-0.65));
#8005=CARTESIAN_POINT('Ctrl Pts',(-0.375277674973257,0.453180457891261,
-0.65));
#8006=CARTESIAN_POINT('Ctrl Pts',(1.66866520601161E-13,0.561513791224244,
-0.65));
#8007=CARTESIAN_POINT('Ctrl Pts',(0.375277674973257,0.45318045789126,-0.65));
#8008=CARTESIAN_POINT('Ctrl Pts',(-0.750555349946514,0.453180457891261,
-9.19165206894919E-17));
#8009=CARTESIAN_POINT('Ctrl Pts',(-0.562916512459802,0.561513791224244,
-0.325000000000144));
#8010=CARTESIAN_POINT('Ctrl Pts',(-0.375277674973257,0.45318045789126,-0.65));
#8011=CARTESIAN_POINT('Origin',(0.375277674973257,0.,-0.65));
#8012=CARTESIAN_POINT('',(0.375277674973257,0.,-0.65));
#8013=CARTESIAN_POINT('',(0.375277674973257,0.,-0.65));
#8014=CARTESIAN_POINT('',(-0.375277674973257,0.,-0.65));
#8015=CARTESIAN_POINT('',(0.375277674973257,0.,-0.65));
#8016=CARTESIAN_POINT('',(-0.375277674973257,0.,-0.65));
#8017=CARTESIAN_POINT('Origin',(0.750555349946514,0.,0.));
#8018=CARTESIAN_POINT('',(0.750555349946514,0.,0.));
#8019=CARTESIAN_POINT('',(0.750555349946514,0.,0.));
#8020=CARTESIAN_POINT('',(0.750555349946514,0.,0.));
#8021=CARTESIAN_POINT('Origin',(0.375277674973257,0.,0.65));
#8022=CARTESIAN_POINT('',(0.375277674973257,0.,0.65));
#8023=CARTESIAN_POINT('',(0.375277674973257,0.,0.65));
#8024=CARTESIAN_POINT('',(0.375277674973257,0.,0.65));
#8025=CARTESIAN_POINT('Origin',(-0.375277674973257,0.,0.65));
#8026=CARTESIAN_POINT('',(-0.375277674973257,0.,0.65));
#8027=CARTESIAN_POINT('',(-0.375277674973257,0.,0.65));
#8028=CARTESIAN_POINT('',(-0.375277674973257,0.,0.65));
#8029=CARTESIAN_POINT('Origin',(-0.750555349946514,0.,-9.19165206894919E-17));
#8030=CARTESIAN_POINT('',(-0.750555349946514,0.,-9.19165206894919E-17));
#8031=CARTESIAN_POINT('',(-0.750555349946514,0.,-9.19165206894919E-17));
#8032=CARTESIAN_POINT('',(-0.750555349946514,0.,-9.19165206894919E-17));
#8033=CARTESIAN_POINT('Origin',(-0.375277674973257,0.,-0.65));
#8034=CARTESIAN_POINT('',(-0.375277674973257,0.,-0.65));
#8035=CARTESIAN_POINT('Origin',(0.,0.53,-1.11022302462516E-16));
#8036=CARTESIAN_POINT('Origin',(0.,0.,-1.11022302462516E-16));
#8037=CARTESIAN_POINT('',(0.,0.,0.));
#8038=CARTESIAN_POINT('Origin',(0.,0.067277284513851,0.));
#8039=CARTESIAN_POINT('',(-0.375277674973257,0.0768195421087395,0.65));
#8040=CARTESIAN_POINT('',(0.375277674973257,0.0768195421087395,0.65));
#8041=CARTESIAN_POINT('Ctrl Pts',(-0.375277674973257,0.0768195421087395,
0.65));
#8042=CARTESIAN_POINT('Ctrl Pts',(1.66533453693773E-13,-0.0315137912242439,
0.65));
#8043=CARTESIAN_POINT('Ctrl Pts',(0.375277674973257,0.0768195421087394,
0.65));
#8044=CARTESIAN_POINT('',(-0.750555349946514,0.0768195421087394,-9.19165206894919E-17));
#8045=CARTESIAN_POINT('Ctrl Pts',(-0.750555349946514,0.0768195421087394,
-9.19165206894919E-17));
#8046=CARTESIAN_POINT('Ctrl Pts',(-0.562916512459802,-0.0315137912242434,
0.325000000000144));
#8047=CARTESIAN_POINT('Ctrl Pts',(-0.375277674973257,0.0768195421087395,
0.65));
#8048=CARTESIAN_POINT('',(-0.6175,-2.77555756156289E-17,-7.5621939847349E-17));
#8049=CARTESIAN_POINT('',(-0.734027674973257,0.067277284513851,-8.98924642641573E-17));
#8050=CARTESIAN_POINT('Origin',(0.,0.,0.));
#8051=CARTESIAN_POINT('',(-0.375277674973257,0.0768195421087395,-0.65));
#8052=CARTESIAN_POINT('Ctrl Pts',(-0.375277674973257,0.0768195421087395,
-0.65));
#8053=CARTESIAN_POINT('Ctrl Pts',(-0.562916512459968,-0.0315137912242437,
-0.324999999999856));
#8054=CARTESIAN_POINT('Ctrl Pts',(-0.750555349946514,0.0768195421087395,
-9.19165206894919E-17));
#8055=CARTESIAN_POINT('',(0.375277674973257,0.0768195421087395,-0.65));
#8056=CARTESIAN_POINT('Ctrl Pts',(0.375277674973257,0.0768195421087395,
-0.65));
#8057=CARTESIAN_POINT('Ctrl Pts',(-1.66144875635155E-13,-0.0315137912242437,
-0.65));
#8058=CARTESIAN_POINT('Ctrl Pts',(-0.375277674973257,0.0768195421087395,
-0.65));
#8059=CARTESIAN_POINT('',(0.750555349946514,0.0768195421087394,0.));
#8060=CARTESIAN_POINT('Ctrl Pts',(0.750555349946514,0.0768195421087394,
0.));
#8061=CARTESIAN_POINT('Ctrl Pts',(0.562916512459802,-0.0315137912242436,
-0.325000000000144));
#8062=CARTESIAN_POINT('Ctrl Pts',(0.375277674973257,0.0768195421087395,
-0.65));
#8063=CARTESIAN_POINT('Ctrl Pts',(0.375277674973257,0.0768195421087394,
0.65));
#8064=CARTESIAN_POINT('Ctrl Pts',(0.562916512459968,-0.0315137912242439,
0.324999999999856));
#8065=CARTESIAN_POINT('Ctrl Pts',(0.750555349946514,0.0768195421087394,
0.));
#8066=CARTESIAN_POINT('Origin',(0.,0.612722715486149,0.));
#8067=CARTESIAN_POINT('',(-0.6175,0.68,-7.5621939847349E-17));
#8068=CARTESIAN_POINT('Origin',(0.,0.68,0.));
#8069=CARTESIAN_POINT('',(-0.750555349946514,0.603180457891261,-9.19165206894919E-17));
#8070=CARTESIAN_POINT('',(-0.734027674973257,0.612722715486149,-8.98924642641573E-17));
#8071=CARTESIAN_POINT('',(-0.375277674973257,0.603180457891261,0.65));
#8072=CARTESIAN_POINT('Ctrl Pts',(-0.375277674973257,0.603180457891261,
0.65));
#8073=CARTESIAN_POINT('Ctrl Pts',(-0.562916512459968,0.711513791224243,
0.324999999999856));
#8074=CARTESIAN_POINT('Ctrl Pts',(-0.750555349946514,0.603180457891261,
-9.19165206894919E-17));
#8075=CARTESIAN_POINT('',(0.375277674973257,0.603180457891261,0.65));
#8076=CARTESIAN_POINT('Ctrl Pts',(0.375277674973257,0.603180457891261,0.65));
#8077=CARTESIAN_POINT('Ctrl Pts',(-1.66755498298699E-13,0.711513791224244,
0.65));
#8078=CARTESIAN_POINT('Ctrl Pts',(-0.375277674973257,0.603180457891261,
0.65));
#8079=CARTESIAN_POINT('',(0.750555349946514,0.603180457891261,0.));
#8080=CARTESIAN_POINT('Ctrl Pts',(0.750555349946514,0.603180457891261,0.));
#8081=CARTESIAN_POINT('Ctrl Pts',(0.562916512459802,0.711513791224244,0.325000000000144));
#8082=CARTESIAN_POINT('Ctrl Pts',(0.375277674973257,0.603180457891261,0.65));
#8083=CARTESIAN_POINT('',(0.375277674973257,0.603180457891261,-0.65));
#8084=CARTESIAN_POINT('Ctrl Pts',(0.375277674973257,0.603180457891261,-0.65));
#8085=CARTESIAN_POINT('Ctrl Pts',(0.562916512459969,0.711513791224244,-0.324999999999856));
#8086=CARTESIAN_POINT('Ctrl Pts',(0.750555349946514,0.603180457891261,0.));
#8087=CARTESIAN_POINT('',(-0.375277674973257,0.603180457891261,-0.65));
#8088=CARTESIAN_POINT('Ctrl Pts',(-0.375277674973257,0.603180457891261,
-0.65));
#8089=CARTESIAN_POINT('Ctrl Pts',(1.66422431391311E-13,0.711513791224244,
-0.65));
#8090=CARTESIAN_POINT('Ctrl Pts',(0.375277674973257,0.603180457891261,-0.65));
#8091=CARTESIAN_POINT('Ctrl Pts',(-0.750555349946514,0.603180457891261,
-9.19165206894919E-17));
#8092=CARTESIAN_POINT('Ctrl Pts',(-0.562916512459802,0.711513791224244,
-0.325000000000144));
#8093=CARTESIAN_POINT('Ctrl Pts',(-0.375277674973257,0.603180457891261,
-0.65));
#8094=CARTESIAN_POINT('Origin',(0.375277674973257,0.,-0.65));
#8095=CARTESIAN_POINT('',(-0.375277674973257,0.,-0.65));
#8096=CARTESIAN_POINT('',(0.375277674973257,0.,-0.65));
#8097=CARTESIAN_POINT('Origin',(-0.375277674973257,0.,-0.65));
#8098=CARTESIAN_POINT('',(-0.750555349946514,0.,-9.19165206894919E-17));
#8099=CARTESIAN_POINT('Origin',(-0.750555349946514,0.,-9.19165206894919E-17));
#8100=CARTESIAN_POINT('',(-0.375277674973257,0.,0.65));
#8101=CARTESIAN_POINT('Origin',(0.,0.,0.));
#8102=CARTESIAN_POINT('',(-0.338975,0.68,4.15124648740974E-17));
#8103=CARTESIAN_POINT('Origin',(0.,0.68,0.));
#8104=CARTESIAN_POINT('',(-0.338975,0.,4.15124648740974E-17));
#8105=CARTESIAN_POINT('',(-0.338975,0.,4.15124648740974E-17));
#8106=CARTESIAN_POINT('Origin',(0.,0.,0.));
#8107=CARTESIAN_POINT('Origin',(-0.375277674973257,0.,0.65));
#8108=CARTESIAN_POINT('',(0.375277674973257,0.,0.65));
#8109=CARTESIAN_POINT('Origin',(0.750555349946514,0.,0.));
#8110=CARTESIAN_POINT('',(0.750555349946514,0.,0.));
#8111=CARTESIAN_POINT('Origin',(0.375277674973257,0.,0.65));
#8112=CARTESIAN_POINT('Origin',(0.,0.68,-1.11022302462516E-16));
#8113=CARTESIAN_POINT('Origin',(0.,0.,-1.11022302462516E-16));
#8114=CARTESIAN_POINT('',(0.,0.,0.));
#8115=CARTESIAN_POINT('Ctrl Pts',(0.872161950711206,0.124828769264236,-0.00589269379913899));
#8116=CARTESIAN_POINT('Ctrl Pts',(0.872090904698941,0.127953657301625,0.0603380612992187));
#8117=CARTESIAN_POINT('Ctrl Pts',(0.857308714561314,0.134203213047992,0.190241275757611));
#8118=CARTESIAN_POINT('Ctrl Pts',(0.770187083636269,0.146690001256174,0.438769378299054));
#8119=CARTESIAN_POINT('Ctrl Pts',(0.560950745207346,0.162256028321672,0.699616259986153));
#8120=CARTESIAN_POINT('Ctrl Pts',(0.199511576340965,0.180880209711553,0.871422024437173));
#8121=CARTESIAN_POINT('Ctrl Pts',(-0.199312333389545,0.199448331926636,
0.868457819907934));
#8122=CARTESIAN_POINT('Ctrl Pts',(-0.556088930421348,0.217951986567579,
0.692928582783942));
#8123=CARTESIAN_POINT('Ctrl Pts',(-0.799862508003898,0.236416030436661,
0.380262416576452));
#8124=CARTESIAN_POINT('Ctrl Pts',(-0.882895646021795,0.254773193569333,
-0.0060546706614528));
#8125=CARTESIAN_POINT('Ctrl Pts',(-0.789649057445972,0.273182184223599,
-0.388883291654368));
#8126=CARTESIAN_POINT('Ctrl Pts',(-0.539659944242912,0.291280837799174,
-0.691764713311758));
#8127=CARTESIAN_POINT('Ctrl Pts',(-0.183956800223335,0.309860445327341,
-0.855316888413074));
#8128=CARTESIAN_POINT('Ctrl Pts',(0.206499015809491,0.327389549600143,-0.847162298078497));
#8129=CARTESIAN_POINT('Ctrl Pts',(0.49509577120488,0.34362645645855,-0.700495805282282));
#8130=CARTESIAN_POINT('Ctrl Pts',(0.670997034604971,0.353943958171212,-0.515417881277946));
#8131=CARTESIAN_POINT('Ctrl Pts',(0.766581438347442,0.365141873832304,-0.355537227212008));
#8132=CARTESIAN_POINT('Ctrl Pts',(0.8174676017473,0.371459915026287,-0.198233634126398));
#8133=CARTESIAN_POINT('Ctrl Pts',(0.834170515466371,0.374539492519685,-0.0771620442826736));
#8134=CARTESIAN_POINT('Ctrl Pts',(0.837719002104484,0.383704512647053,0.0354460071939376));
#8135=CARTESIAN_POINT('Ctrl Pts',(0.817405541799073,0.413175723298386,0.185924750839524));
#8136=CARTESIAN_POINT('Ctrl Pts',(0.748423543506377,0.44312071842525,0.367957985006333));
#8137=CARTESIAN_POINT('Ctrl Pts',(0.647340094288683,0.470691270109384,0.518903872562794));
#8138=CARTESIAN_POINT('Ctrl Pts',(0.466898254116811,0.511144063135416,0.691309623343175));
#8139=CARTESIAN_POINT('Ctrl Pts',(0.182800989155019,0.558222951408999,0.818397523700333));
#8140=CARTESIAN_POINT('Ctrl Pts',(-0.189545178060892,0.616501258086875,
0.809773850041606));
#8141=CARTESIAN_POINT('Ctrl Pts',(-0.462507583347405,0.663503908067788,
0.669357773844709));
#8142=CARTESIAN_POINT('Ctrl Pts',(-0.627863189228003,0.701318402481341,
0.495969553901588));
#8143=CARTESIAN_POINT('Ctrl Pts',(-0.750267427503473,0.738837453517587,
0.291088758101646));
#8144=CARTESIAN_POINT('Ctrl Pts',(-0.810712868559922,0.785528896923523,
-0.00492588128797676));
#8145=CARTESIAN_POINT('Ctrl Pts',(-0.722807305049749,0.841109138477463,
-0.35397737605765));
#8146=CARTESIAN_POINT('Ctrl Pts',(-0.493845277109899,0.896322143289524,
-0.6284699970223));
#8147=CARTESIAN_POINT('Ctrl Pts',(-0.170668331595556,0.951180240767939,
-0.77578162036287));
#8148=CARTESIAN_POINT('Ctrl Pts',(0.182411368712431,1.00572789901627,-0.768554583075931));
#8149=CARTESIAN_POINT('Ctrl Pts',(0.495894675031221,1.0599979812032,-0.609891173973463));
#8150=CARTESIAN_POINT('Ctrl Pts',(0.708755333326572,1.11403086100534,-0.332295680974433));
#8151=CARTESIAN_POINT('Ctrl Pts',(0.780070637830783,1.16786510347237,0.00885468431853584));
#8152=CARTESIAN_POINT('Ctrl Pts',(0.696791510479646,1.22154183082612,0.346232027663686));
#8153=CARTESIAN_POINT('Ctrl Pts',(0.476047266626745,1.27510240963086,0.61364355273423));
#8154=CARTESIAN_POINT('Ctrl Pts',(0.161678386661078,1.32858888114584,0.758820094473604));
#8155=CARTESIAN_POINT('Ctrl Pts',(-0.184345221885054,1.38204344182885,0.753472314023915));
#8156=CARTESIAN_POINT('Ctrl Pts',(-0.493955884546455,1.43550888318168,0.598711183433611));
#8157=CARTESIAN_POINT('Ctrl Pts',(-0.706164418456796,1.48902767046263,0.324820470310737));
#8158=CARTESIAN_POINT('Ctrl Pts',(-0.778894190579621,1.54264192169839,-0.0145743797186695));
#8159=CARTESIAN_POINT('Ctrl Pts',(-0.697192877485004,1.59639341722752,-0.352835018065878));
#8160=CARTESIAN_POINT('Ctrl Pts',(-0.476282548914222,1.65032345266182,-0.623209180930827));
#8161=CARTESIAN_POINT('Ctrl Pts',(-0.158743612035258,1.70447207761938,-0.771770092812482));
#8162=CARTESIAN_POINT('Ctrl Pts',(0.193450677004803,1.75887837965647,-0.768113401787862));
#8163=CARTESIAN_POINT('Ctrl Pts',(0.47579440943534,1.80750241451549,-0.628734440560694));
#8164=CARTESIAN_POINT('Ctrl Pts',(0.659272267850805,1.85026369378763,-0.426676852570877));
#8165=CARTESIAN_POINT('Ctrl Pts',(0.793229432459306,1.89934423589563,-0.143355198493509));
#8166=CARTESIAN_POINT('Ctrl Pts',(0.790263784307131,1.96111512092083,0.264407243055348));
#8167=CARTESIAN_POINT('Ctrl Pts',(0.532639208585251,2.02974904747753,0.637020032041957));
#8168=CARTESIAN_POINT('Ctrl Pts',(0.163609475192015,2.09273970975414,0.811198964310618));
#8169=CARTESIAN_POINT('Ctrl Pts',(-0.206325324489528,2.14991769756873,0.809290051602918));
#8170=CARTESIAN_POINT('Ctrl Pts',(-0.54210311156644,2.20760646525503,0.645493293137588));
#8171=CARTESIAN_POINT('Ctrl Pts',(-0.775793177879044,2.26582771180786,0.349801965195082));
#8172=CARTESIAN_POINT('Ctrl Pts',(-0.859118193146955,2.32460053758821,-0.0214433086745682));
#8173=CARTESIAN_POINT('Ctrl Pts',(-0.772497333242961,2.38394137391289,-0.395836964477112));
#8174=CARTESIAN_POINT('Ctrl Pts',(-0.529877815574135,2.44386394296014,-0.698375208084907));
#8175=CARTESIAN_POINT('Ctrl Pts',(-0.137454124419672,2.51110274201743,-0.887126219786336));
#8176=CARTESIAN_POINT('Ctrl Pts',(0.355020405406913,2.58592160387692,-0.85044216028401));
#8177=CARTESIAN_POINT('Ctrl Pts',(0.782180417385646,2.66862024366749,-0.50996194705241));
#8178=CARTESIAN_POINT('Ctrl Pts',(0.932029131507338,2.74541647960869,-0.0258957186176781));
#8179=CARTESIAN_POINT('Ctrl Pts',(0.830321215974015,2.81601192011723,0.419957402046343));
#8180=CARTESIAN_POINT('Ctrl Pts',(0.572400166827825,2.88014282443316,0.744989944459363));
#8181=CARTESIAN_POINT('Ctrl Pts',(0.195275509838113,2.94485897026784,0.927771382562365));
#8182=CARTESIAN_POINT('Ctrl Pts',(-0.227340767365424,3.01014754818103,0.929095017890615));
#8183=CARTESIAN_POINT('Ctrl Pts',(-0.612127646814787,3.07599293903656,0.745588291188903));
#8184=CARTESIAN_POINT('Ctrl Pts',(-0.881535208369304,3.14237676662695,0.410744646425331));
#8185=CARTESIAN_POINT('Ctrl Pts',(-0.980005185206354,3.20927820175596,-0.0110388926131081));
#8186=CARTESIAN_POINT('Ctrl Pts',(-0.885263395772081,3.27667359822412,-0.436952466191731));
#8187=CARTESIAN_POINT('Ctrl Pts',(-0.613436538369041,3.34453700325931,-0.782121048029494));
#8188=CARTESIAN_POINT('Ctrl Pts',(-0.216315847404239,3.41284022102408,-0.976638893510757));
#8189=CARTESIAN_POINT('Ctrl Pts',(0.228515688692952,3.48155290325642,-0.979879367890244));
#8190=CARTESIAN_POINT('Ctrl Pts',(0.633032334246116,3.55064249055004,-0.788946617304531));
#8191=CARTESIAN_POINT('Ctrl Pts',(0.91620307923501,3.62007471455624,-0.439929095068272));
#8192=CARTESIAN_POINT('Ctrl Pts',(1.02068551154318,3.6898138200776,-0.00055988972616793));
#8193=CARTESIAN_POINT('Ctrl Pts',(0.923874643413053,3.75982214337787,0.441983752855437));
#8194=CARTESIAN_POINT('Ctrl Pts',(0.613247660943624,3.83786518922612,0.840785019888275));
#8195=CARTESIAN_POINT('Ctrl Pts',(0.0866578234258063,3.9239844102579,1.05456997463629));
#8196=CARTESIAN_POINT('Ctrl Pts',(-0.521392660403112,4.01817435387289,0.92294994186792));
#8197=CARTESIAN_POINT('Ctrl Pts',(-0.914636612404499,4.10464567111125,0.509573712510557));
#8198=CARTESIAN_POINT('Ctrl Pts',(-1.03374180999006,4.18328650371776,0.0141535738014065));
#8199=CARTESIAN_POINT('Ctrl Pts',(-0.938026942329867,4.25404428614242,-0.433573776623787));
#8200=CARTESIAN_POINT('Ctrl Pts',(-0.657630260146868,4.32474041714926,-0.795496981882739));
#8201=CARTESIAN_POINT('Ctrl Pts',(-0.294187702113077,4.38748944604847,-0.977023505420508));
#8202=CARTESIAN_POINT('Ctrl Pts',(0.0542596632323615,4.44230054898675,-1.00807090756588));
#8203=CARTESIAN_POINT('Ctrl Pts',(0.445198581282316,4.50483969839108,-0.926094625208896));
#8204=CARTESIAN_POINT('Ctrl Pts',(0.852563310440807,4.58279123657346,-0.611941112564204));
#8205=CARTESIAN_POINT('Ctrl Pts',(1.04336115553597,4.67588518836249,-0.0274765552718303));
#8206=CARTESIAN_POINT('Ctrl Pts',(0.873243552350396,4.76843871793217,0.559396655291762));
#8207=CARTESIAN_POINT('Ctrl Pts',(0.405532574611691,4.86037265153526,0.946224142384314));
#8208=CARTESIAN_POINT('Ctrl Pts',(-0.194232561825003,4.95159408982323,1.00246182575268));
#8209=CARTESIAN_POINT('Ctrl Pts',(-0.716978005254575,5.04205915598986,0.713684974901636));
#8210=CARTESIAN_POINT('Ctrl Pts',(-0.984237521133288,5.13163619116299,0.185945073380498));
#8211=CARTESIAN_POINT('Ctrl Pts',(-0.909022704364039,5.22040809154829,-0.394980663551699));
#8212=CARTESIAN_POINT('Ctrl Pts',(-0.524008362921299,5.30799616173538,-0.827628543573509));
#8213=CARTESIAN_POINT('Ctrl Pts',(0.0311612934979211,5.39510126764713,-0.968284503878036));
#8214=CARTESIAN_POINT('Ctrl Pts',(0.452486451456519,5.46227744588555,-0.812413771015693));
#8215=CARTESIAN_POINT('Ctrl Pts',(0.678996914481602,5.51263767773254,-0.597335976683866));
#8216=CARTESIAN_POINT('Ctrl Pts',(0.792756702852497,5.54424482065645,-0.425194580715441));
#8217=CARTESIAN_POINT('Ctrl Pts',(0.861097079444627,5.57344984716716,-0.244943323368279));
#8218=CARTESIAN_POINT('Ctrl Pts',(0.885548394683697,5.6069898998326,-0.0758116878038518));
#8219=CARTESIAN_POINT('Ctrl Pts',(0.881311178103886,5.61908885250671,0.0702661570768112));
#8220=CARTESIAN_POINT('Ctrl Pts',(0.861324400417122,5.62225654974902,0.205633030471336));
#8221=CARTESIAN_POINT('Ctrl Pts',(0.812891366893097,5.62852110126019,0.357273663598819));
#8222=CARTESIAN_POINT('Ctrl Pts',(0.709033945858278,5.64053429758327,0.532105911493553));
#8223=CARTESIAN_POINT('Ctrl Pts',(0.526480038594941,5.65124067536637,0.723242801555853));
#8224=CARTESIAN_POINT('Ctrl Pts',(0.225331281496905,5.66829963228703,0.876812377650357));
#8225=CARTESIAN_POINT('Ctrl Pts',(-0.178438754359568,5.6861889761217,0.884400172818289));
#8226=CARTESIAN_POINT('Ctrl Pts',(-0.544244744848784,5.70539124964099,0.716342713969011));
#8227=CARTESIAN_POINT('Ctrl Pts',(-0.799436178683323,5.72389218103035,0.406445379440496));
#8228=CARTESIAN_POINT('Ctrl Pts',(-0.893901515434013,5.74261482334007,0.0176118727011753));
#8229=CARTESIAN_POINT('Ctrl Pts',(-0.809793026073925,5.76114914213192,-0.372336066624544));
#8230=CARTESIAN_POINT('Ctrl Pts',(-0.565009292976944,5.77968086993593,-0.685823620580416));
#8231=CARTESIAN_POINT('Ctrl Pts',(-0.209171565907703,5.79813086800354,-0.860593511818846));
#8232=CARTESIAN_POINT('Ctrl Pts',(0.186034384156284,5.8165319894943,-0.863241242665013));
#8233=CARTESIAN_POINT('Ctrl Pts',(0.541844299347737,5.83487223159308,-0.693819904186464));
#8234=CARTESIAN_POINT('Ctrl Pts',(0.746471713940332,5.85010991085684,-0.43833815015316));
#8235=CARTESIAN_POINT('Ctrl Pts',(0.831270497111571,5.86227119228351,-0.19628398706425));
#8236=CARTESIAN_POINT('Ctrl Pts',(0.845616258369985,5.86833999900766,-0.0701367303899257));
#8237=CARTESIAN_POINT('Ctrl Pts',(0.845685384742026,5.87138045372904,-0.00569550566726366));
#8238=CARTESIAN_POINT('Ctrl Pts',(0.834771700518231,0.123978681791665,-0.00589269379913899));
#8239=CARTESIAN_POINT('Ctrl Pts',(0.834703585425039,0.126974656274918,0.0576057899568015));
#8240=CARTESIAN_POINT('Ctrl Pts',(0.820566864806215,0.132951747306104,0.1818462773769));
#8241=CARTESIAN_POINT('Ctrl Pts',(0.737159418128638,0.144907869145536,0.41981635707622));
#8242=CARTESIAN_POINT('Ctrl Pts',(0.536913029824937,0.159802973361417,0.669408868982891));
#8243=CARTESIAN_POINT('Ctrl Pts',(0.19099562145444,0.177628187211079,0.833856980367138));
#8244=CARTESIAN_POINT('Ctrl Pts',(-0.190655324048718,0.195396044249228,
0.830996898689714));
#8245=CARTESIAN_POINT('Ctrl Pts',(-0.53207161478927,0.213103379696006,0.663031596529677));
#8246=CARTESIAN_POINT('Ctrl Pts',(-0.765333292231674,0.230771512020908,
0.36382917330982));
#8247=CARTESIAN_POINT('Ctrl Pts',(-0.844788059380974,0.248338044161933,
-0.00584534341205808));
#8248=CARTESIAN_POINT('Ctrl Pts',(-0.755550469517709,0.265954744653817,
-0.372189649298638));
#8249=CARTESIAN_POINT('Ctrl Pts',(-0.516314131999674,0.283275239097253,
-0.662046752944101));
#8250=CARTESIAN_POINT('Ctrl Pts',(-0.175874814910529,0.301058416266183,
-0.818563370277865));
#8251=CARTESIAN_POINT('Ctrl Pts',(0.197837874836819,0.317836237075745,-0.810772944672516));
#8252=CARTESIAN_POINT('Ctrl Pts',(0.474117448088369,0.333381343729803,-0.670340422853212));
#8253=CARTESIAN_POINT('Ctrl Pts',(0.642476318144299,0.343257359612203,-0.493219944846032));
#8254=CARTESIAN_POINT('Ctrl Pts',(0.734084644784475,0.353986453186565,-0.339953181467585));
#8255=CARTESIAN_POINT('Ctrl Pts',(0.782670889327258,0.360026050725482,-0.189705341255422));
#8256=CARTESIAN_POINT('Ctrl Pts',(0.798724557788542,0.362974904968381,-0.0735631332743304));
#8257=CARTESIAN_POINT('Ctrl Pts',(0.802141543715252,0.371811933026709,0.0349840749294869));
#8258=CARTESIAN_POINT('Ctrl Pts',(0.782571839931757,0.400140924438028,0.179601073342154));
#8259=CARTESIAN_POINT('Ctrl Pts',(0.716586436607174,0.428773049861363,0.353720744375737));
#8260=CARTESIAN_POINT('Ctrl Pts',(0.619452048298751,0.455282772577966,0.498840903387784));
#8261=CARTESIAN_POINT('Ctrl Pts',(0.446338986242718,0.494085589245527,0.664198743741128));
#8262=CARTESIAN_POINT('Ctrl Pts',(0.173348026654919,0.539339087364759,0.786420950987734));
#8263=CARTESIAN_POINT('Ctrl Pts',(-0.184821452882668,0.595395544254175,
0.778115761403682));
#8264=CARTESIAN_POINT('Ctrl Pts',(-0.447871399056696,0.640697053109364,
0.642894143294883));
#8265=CARTESIAN_POINT('Ctrl Pts',(-0.607392342756213,0.677176186867957,
0.47562801903027));
#8266=CARTESIAN_POINT('Ctrl Pts',(-0.725592115215377,0.713406676016781,
0.277808215850071));
#8267=CARTESIAN_POINT('Ctrl Pts',(-0.784113311361799,0.758571100411465,
-0.0084746015749381));
#8268=CARTESIAN_POINT('Ctrl Pts',(-0.698996863957015,0.812438504258161,
-0.346766060602901));
#8269=CARTESIAN_POINT('Ctrl Pts',(-0.476612351424375,0.866092299597088,
-0.613526369115138));
#8270=CARTESIAN_POINT('Ctrl Pts',(-0.161859501263566,0.919532790752191,
-0.757098553956881));
#8271=CARTESIAN_POINT('Ctrl Pts',(0.183015403440875,0.972820718761726,-0.750147817033866));
#8272=CARTESIAN_POINT('Ctrl Pts',(0.490154877552902,1.02599129588717,-0.59481688084477));
#8273=CARTESIAN_POINT('Ctrl Pts',(0.699403601519287,1.07909221978425,-0.322121854432755));
#8274=CARTESIAN_POINT('Ctrl Pts',(0.769817441643044,1.13216585492274,0.0141331161359554));
#8275=CARTESIAN_POINT('Ctrl Pts',(0.687578814649516,1.18525747666464,0.347809311925023));
#8276=CARTESIAN_POINT('Ctrl Pts',(0.468644093923167,1.23841119165469,0.613227239522894));
#8277=CARTESIAN_POINT('Ctrl Pts',(0.155712125133277,1.29167111889997,0.757881850017962));
#8278=CARTESIAN_POINT('Ctrl Pts',(-0.189963695061651,1.34508056439839,0.752669618582056));
#8279=CARTESIAN_POINT('Ctrl Pts',(-0.500371056919822,1.39868255819304,0.597656322850705));
#8280=CARTESIAN_POINT('Ctrl Pts',(-0.713905011413384,1.45251897515664,0.322267362968876));
#8281=CARTESIAN_POINT('Ctrl Pts',(-0.787422097915162,1.50663031435001,-0.0201881452818813));
#8282=CARTESIAN_POINT('Ctrl Pts',(-0.70483144226016,1.56105630602259,-0.362661071536256));
#8283=CARTESIAN_POINT('Ctrl Pts',(-0.480579928801225,1.61583446556222,-0.637316626417315));
#8284=CARTESIAN_POINT('Ctrl Pts',(-0.157171190478558,1.67100240976954,-0.788747246876486));
#8285=CARTESIAN_POINT('Ctrl Pts',(0.202622739833848,1.7265916485172,-0.785124172182557));
#8286=CARTESIAN_POINT('Ctrl Pts',(0.491912328391669,1.77641473527713,-0.642420818797231));
#8287=CARTESIAN_POINT('Ctrl Pts',(0.680285980292682,1.82031497486235,-0.435026313679016));
#8288=CARTESIAN_POINT('Ctrl Pts',(0.818038947603602,1.87077846101778,-0.143766162147066));
#8289=CARTESIAN_POINT('Ctrl Pts',(0.815175070026228,1.93444545082108,0.276468601290314));
#8290=CARTESIAN_POINT('Ctrl Pts',(0.549116837182812,2.00536570374533,0.661583099652164));
#8291=CARTESIAN_POINT('Ctrl Pts',(0.167011133590032,2.07060227586673,0.842042743615258));
#8292=CARTESIAN_POINT('Ctrl Pts',(-0.21668597901319,2.12991550296718,0.840139239691205));
#8293=CARTESIAN_POINT('Ctrl Pts',(-0.56542563851628,2.18983288558837,0.670094225008614));
#8294=CARTESIAN_POINT('Ctrl Pts',(-0.808434298594091,2.25037079909405,0.362707877766159));
#8295=CARTESIAN_POINT('Ctrl Pts',(-0.895185566716189,2.31153566652781,-0.0236000562992145));
#8296=CARTESIAN_POINT('Ctrl Pts',(-0.805022512927831,2.37333259941659,-0.413465766229975));
#8297=CARTESIAN_POINT('Ctrl Pts',(-0.552281502791154,2.43576574672377,-0.728669680768865));
#8298=CARTESIAN_POINT('Ctrl Pts',(-0.143381208770228,2.50583018408946,-0.925360181836486));
#8299=CARTESIAN_POINT('Ctrl Pts',(0.369825525208484,2.58380175548622,-0.887137157875364));
#8300=CARTESIAN_POINT('Ctrl Pts',(0.814804343279841,2.66995453964888,-0.532409524853484));
#8301=CARTESIAN_POINT('Ctrl Pts',(0.970765313247155,2.74990885053001,-0.0284299122440809));
#8302=CARTESIAN_POINT('Ctrl Pts',(0.864935389584109,2.82334491449737,0.435356252438035));
#8303=CARTESIAN_POINT('Ctrl Pts',(0.596849899496631,2.88999636123757,0.773145656467097));
#8304=CARTESIAN_POINT('Ctrl Pts',(0.205293441378129,2.95718454933558,0.962873173642001));
#8305=CARTESIAN_POINT('Ctrl Pts',(-0.232943838476479,3.0248846278283,0.964194207817526));
#8306=CARTESIAN_POINT('Ctrl Pts',(-0.631388236736662,3.09306905210793,0.774108113890306));
#8307=CARTESIAN_POINT('Ctrl Pts',(-0.909907742648915,3.16170797304782,0.427832174748424));
#8308=CARTESIAN_POINT('Ctrl Pts',(-1.01149030028913,3.23076953302768,-0.00760996058240064));
#8309=CARTESIAN_POINT('Ctrl Pts',(-0.913775364912534,3.30021940688078,-0.446516565593066));
#8310=CARTESIAN_POINT('Ctrl Pts',(-0.634094793286599,3.37002153658447,-0.801516768025116));
#8311=CARTESIAN_POINT('Ctrl Pts',(-0.226357821320832,3.4401382001316,-1.00113129709783));
#8312=CARTESIAN_POINT('Ctrl Pts',(0.229385441734438,3.51053009248794,-1.00435311710641));
#8313=CARTESIAN_POINT('Ctrl Pts',(0.642894477389595,3.581156328932,-0.809062746948213));
#8314=CARTESIAN_POINT('Ctrl Pts',(0.931669474071348,3.65197488117754,-0.452972351757245));
#8315=CARTESIAN_POINT('Ctrl Pts',(1.03789787376058,3.72294319562607,-0.00578432429799382));
#8316=CARTESIAN_POINT('Ctrl Pts',(0.939501321407795,3.79401668275829,0.443524276145958));
#8317=CARTESIAN_POINT('Ctrl Pts',(0.62476031217733,3.87305514732048,0.847385644602313));
#8318=CARTESIAN_POINT('Ctrl Pts',(0.0927824485508912,3.96002981676028,1.06307663026052));
#8319=CARTESIAN_POINT('Ctrl Pts',(-0.519261103648405,4.05484139765325,0.930258619011824));
#8320=CARTESIAN_POINT('Ctrl Pts',(-0.913615764923826,4.14159563870383,0.515316188012155));
#8321=CARTESIAN_POINT('Ctrl Pts',(-1.03259539479936,4.22024766361548,0.0197349878659042));
#8322=CARTESIAN_POINT('Ctrl Pts',(-0.936985021298801,4.29082468340848,-0.426901854675045));
#8323=CARTESIAN_POINT('Ctrl Pts',(-0.657842936611053,4.36116731303318,-0.78698353983026));
#8324=CARTESIAN_POINT('Ctrl Pts',(-0.29706363491301,4.42343562231095,-0.967045529816717));
#8325=CARTESIAN_POINT('Ctrl Pts',(0.048089905369423,4.47772349208189,-0.997758532861414));
#8326=CARTESIAN_POINT('Ctrl Pts',(0.434672946626173,4.53955785964178,-0.91663997594521));
#8327=CARTESIAN_POINT('Ctrl Pts',(0.836338179989597,4.61643768531908,-0.606572728149323));
#8328=CARTESIAN_POINT('Ctrl Pts',(1.02363261661145,4.70795057452343,-0.0318742450840044));
#8329=CARTESIAN_POINT('Ctrl Pts',(0.856646027640753,4.79864210207537,0.543182406487656));
#8330=CARTESIAN_POINT('Ctrl Pts',(0.399518272233148,4.88845129456705,0.920894696277978));
#8331=CARTESIAN_POINT('Ctrl Pts',(-0.184736991833155,4.97729888029892,0.97542191054148));
#8332=CARTESIAN_POINT('Ctrl Pts',(-0.692427413956977,5.06517207449486,0.694672374006644));
#8333=CARTESIAN_POINT('Ctrl Pts',(-0.951170369249242,5.15195437290911,0.183262220477753));
#8334=CARTESIAN_POINT('Ctrl Pts',(-0.87826921068102,5.23774553596991,-0.37821229083323));
#8335=CARTESIAN_POINT('Ctrl Pts',(-0.506794241817076,5.32221810148529,-0.795337281353065));
#8336=CARTESIAN_POINT('Ctrl Pts',(0.0276185714897006,5.406047337515,-0.930628214623325));
#8337=CARTESIAN_POINT('Ctrl Pts',(0.432533063223502,5.47061960053111,-0.780638115606707));
#8338=CARTESIAN_POINT('Ctrl Pts',(0.649902755493398,5.51893798204238,-0.574289574590299));
#8339=CARTESIAN_POINT('Ctrl Pts',(0.759237064104118,5.5493319389142,-0.408764864910009));
#8340=CARTESIAN_POINT('Ctrl Pts',(0.824596080015948,5.5772473038315,-0.236380043413035));
#8341=CARTESIAN_POINT('Ctrl Pts',(0.848146928563698,5.60949307144751,-0.0738121405935497));
#8342=CARTESIAN_POINT('Ctrl Pts',(0.844064325097165,5.62115590174748,0.0669803668858104));
#8343=CARTESIAN_POINT('Ctrl Pts',(0.824845436961386,5.62418839323027,0.196889811486777));
#8344=CARTESIAN_POINT('Ctrl Pts',(0.778623685751031,5.63017376408778,0.341659870964739));
#8345=CARTESIAN_POINT('Ctrl Pts',(0.679045301159248,5.64168668150034,0.509321418625131));
#8346=CARTESIAN_POINT('Ctrl Pts',(0.504281215772623,5.65193561221424,0.6922654991445));
#8347=CARTESIAN_POINT('Ctrl Pts',(0.215920333627058,5.66826890972612,0.839327880648377));
#8348=CARTESIAN_POINT('Ctrl Pts',(-0.17059735528807,5.68539243143367,0.846555779303511));
#8349=CARTESIAN_POINT('Ctrl Pts',(-0.52074345759163,5.70377212295289,0.685690634545263));
#8350=CARTESIAN_POINT('Ctrl Pts',(-0.76497770643086,5.7214785814209,0.389076426270338));
#8351=CARTESIAN_POINT('Ctrl Pts',(-0.855376950074861,5.73939616186927,0.0169517243609489));
#8352=CARTESIAN_POINT('Ctrl Pts',(-0.774879778839863,5.75713267952773,-0.356215682043892));
#8353=CARTESIAN_POINT('Ctrl Pts',(-0.540635276851386,5.77486575773549,-0.656201303963563));
#8354=CARTESIAN_POINT('Ctrl Pts',(-0.200120542834017,5.79252128061077,-0.823432503136215));
#8355=CARTESIAN_POINT('Ctrl Pts',(0.178054805747909,5.8101288140521,-0.825978016619043));
#8356=CARTESIAN_POINT('Ctrl Pts',(0.518555465070368,5.82768087002016,-0.663820021983919));
#8357=CARTESIAN_POINT('Ctrl Pts',(0.714370484503248,5.84226048424649,-0.419381891085474));
#8358=CARTESIAN_POINT('Ctrl Pts',(0.795543670584242,5.85390333769986,-0.187643319757738));
#8359=CARTESIAN_POINT('Ctrl Pts',(0.809262236615181,5.85970651710405,-0.067017040736679));
#8360=CARTESIAN_POINT('Ctrl Pts',(0.809328501647431,5.8626211186406,-0.00524322405284286));
#8361=CARTESIAN_POINT('Ctrl Pts',(0.761047787275267,0.0865318839626108,
-0.00420496941242302));
#8362=CARTESIAN_POINT('Ctrl Pts',(0.760985430150483,0.0892745999444253,
0.0539258014575904));
#8363=CARTESIAN_POINT('Ctrl Pts',(0.748119724422766,0.0947160261358312,
0.167035838010278));
#8364=CARTESIAN_POINT('Ctrl Pts',(0.671994482225062,0.105632770703035,0.384332182947992));
#8365=CARTESIAN_POINT('Ctrl Pts',(0.489222617092547,0.119226067914075,0.612118953075658));
#8366=CARTESIAN_POINT('Ctrl Pts',(0.173126210138464,0.135516755152735,0.762481827893436));
#8367=CARTESIAN_POINT('Ctrl Pts',(-0.17591786072793,0.151764656414447,0.759870679153006));
#8368=CARTESIAN_POINT('Ctrl Pts',(-0.488518080787529,0.167976188775447,
0.60615013690747));
#8369=CARTESIAN_POINT('Ctrl Pts',(-0.702300823925886,0.184164859419497,
0.331985628674946));
#8370=CARTESIAN_POINT('Ctrl Pts',(-0.775245837906118,0.20027867376939,-0.00713875728997948));
#8371=CARTESIAN_POINT('Ctrl Pts',(-0.693331186380063,0.216456574823254,
-0.343586819420473));
#8372=CARTESIAN_POINT('Ctrl Pts',(-0.473431441508657,0.232378967624498,
-0.610158028488542));
#8373=CARTESIAN_POINT('Ctrl Pts',(-0.160033292746761,0.248749689057296,
-0.754231386377503));
#8374=CARTESIAN_POINT('Ctrl Pts',(0.184381060038689,0.264211029038414,-0.747212343204508));
#8375=CARTESIAN_POINT('Ctrl Pts',(0.439494987793935,0.278562347450618,-0.617438290361299));
#8376=CARTESIAN_POINT('Ctrl Pts',(0.594761749184093,0.287671299007321,-0.454293092965716));
#8377=CARTESIAN_POINT('Ctrl Pts',(0.680179375188791,0.297642085136332,-0.311159344468621));
#8378=CARTESIAN_POINT('Ctrl Pts',(0.72410263440118,0.303148875483543,-0.17497012052153));
#8379=CARTESIAN_POINT('Ctrl Pts',(0.739436405987218,0.305864048225509,-0.065903096066576));
#8380=CARTESIAN_POINT('Ctrl Pts',(0.742714414172589,0.31452571142108,0.0400611631273491));
#8381=CARTESIAN_POINT('Ctrl Pts',(0.723921821344288,0.341324092131815,0.176490370677569));
#8382=CARTESIAN_POINT('Ctrl Pts',(0.663642989059462,0.367388684091378,0.335525251497113));
#8383=CARTESIAN_POINT('Ctrl Pts',(0.572000817055734,0.392510940637376,0.472934409398862));
#8384=CARTESIAN_POINT('Ctrl Pts',(0.41054956588088,0.428642412363889,0.626837468469602));
#8385=CARTESIAN_POINT('Ctrl Pts',(0.15354749226292,0.471323551336263,0.742522500650089));
#8386=CARTESIAN_POINT('Ctrl Pts',(-0.184911165258365,0.52423475364142,0.734508163497739));
#8387=CARTESIAN_POINT('Ctrl Pts',(-0.435471199252404,0.56738518488992,0.606191945550898));
#8388=CARTESIAN_POINT('Ctrl Pts',(-0.588079297608022,0.602267720216433,
0.446158216855588));
#8389=CARTESIAN_POINT('Ctrl Pts',(-0.701585525374809,0.637046993340004,
0.256315862648341));
#8390=CARTESIAN_POINT('Ctrl Pts',(-0.758246999238167,0.680601831991576,
-0.0198107154225673));
#8391=CARTESIAN_POINT('Ctrl Pts',(-0.67581747589741,0.732951768293531,-0.348648501705937));
#8392=CARTESIAN_POINT('Ctrl Pts',(-0.458356924520715,0.785453130585882,
-0.609932960571064));
#8393=CARTESIAN_POINT('Ctrl Pts',(-0.148060077521017,0.8381505627929,-0.75180328824606));
#8394=CARTESIAN_POINT('Ctrl Pts',(0.194648602326754,0.891090429842906,-0.74518574293805));
#8395=CARTESIAN_POINT('Ctrl Pts',(0.502306763187505,0.944317348882362,-0.589925789789185));
#8396=CARTESIAN_POINT('Ctrl Pts',(0.713634675628132,0.997875028872795,-0.315003755248991));
#8397=CARTESIAN_POINT('Ctrl Pts',(0.785485102314095,1.051805127184,0.0266887056339002));
#8398=CARTESIAN_POINT('Ctrl Pts',(0.701568173162039,1.10614794715317,0.368370321572409));
#8399=CARTESIAN_POINT('Ctrl Pts',(0.476045494703238,1.1609417180984,0.642213034060343));
#8400=CARTESIAN_POINT('Ctrl Pts',(0.151284968811604,1.21622234017789,0.792632503395218));
#8401=CARTESIAN_POINT('Ctrl Pts',(-0.20994906929914,1.27202327147521,0.787444219944241));
#8402=CARTESIAN_POINT('Ctrl Pts',(-0.536462340262496,1.32837570512521,0.624662675732468));
#8403=CARTESIAN_POINT('Ctrl Pts',(-0.762505777513781,1.38530791222031,0.333519162029373));
#8404=CARTESIAN_POINT('Ctrl Pts',(-0.840905814264777,1.4428452883087,-0.0306479907520013));
#8405=CARTESIAN_POINT('Ctrl Pts',(-0.752819154390827,1.50101033643261,-0.396772374613101));
#8406=CARTESIAN_POINT('Ctrl Pts',(-0.512148554946034,1.55982256369068,-0.691829494739243));
#8407=CARTESIAN_POINT('Ctrl Pts',(-0.163487647715867,1.61929805770311,-0.855273682981701));
#8408=CARTESIAN_POINT('Ctrl Pts',(0.225906877040415,1.67944986134947,-0.85149921851126));
#8409=CARTESIAN_POINT('Ctrl Pts',(0.540022411129438,1.73352770394763,-0.696678959007169));
#8410=CARTESIAN_POINT('Ctrl Pts',(0.745035426037874,1.78129469019987,-0.47100411639915));
#8411=CARTESIAN_POINT('Ctrl Pts',(0.895228236006619,1.83629699527816,-0.153554506686288));
#8412=CARTESIAN_POINT('Ctrl Pts',(0.89223927295861,1.90582241797352,0.305405109016149));
#8413=CARTESIAN_POINT('Ctrl Pts',(0.601186880623915,1.98342811819678,0.726898276477956));
#8414=CARTESIAN_POINT('Ctrl Pts',(0.182706367734971,2.05486560581464,0.924537453077089));
#8415=CARTESIAN_POINT('Ctrl Pts',(-0.237609869111216,2.11983305006345,0.922431795780973));
#8416=CARTESIAN_POINT('Ctrl Pts',(-0.619591863889922,2.18545817037548,0.736139114456955));
#8417=CARTESIAN_POINT('Ctrl Pts',(-0.885570229363876,2.25172476080031,0.399599069489404));
#8418=CARTESIAN_POINT('Ctrl Pts',(-0.980372360862589,2.31861247300258,-0.0228969605362083));
#8419=CARTESIAN_POINT('Ctrl Pts',(-0.881808807432037,2.38609753937237,-0.448648878205793));
#8420=CARTESIAN_POINT('Ctrl Pts',(-0.606198581990288,2.45415533882294,-0.792189601098245));
#8421=CARTESIAN_POINT('Ctrl Pts',(-0.161322178004925,2.53037145581947,-1.00603161350487));
#8422=CARTESIAN_POINT('Ctrl Pts',(0.395299379371196,2.61494109989725,-0.964252877413945));
#8423=CARTESIAN_POINT('Ctrl Pts',(0.875781410044385,2.70801792789744,-0.580702867265662));
#8424=CARTESIAN_POINT('Ctrl Pts',(1.04313455820602,2.79401491131878,-0.0385318102786846));
#8425=CARTESIAN_POINT('Ctrl Pts',(0.929559356135266,2.87266356126334,0.458076873271283));
#8426=CARTESIAN_POINT('Ctrl Pts',(0.643431418456286,2.94376259155564,0.81825259369129));
#8427=CARTESIAN_POINT('Ctrl Pts',(0.227420031512275,3.0151340339755,1.01956294456111));
#8428=CARTESIAN_POINT('Ctrl Pts',(-0.236013305313231,3.08673230669762,1.02071321244897));
#8429=CARTESIAN_POINT('Ctrl Pts',(-0.655312712092223,3.15851088990362,0.82039134401966));
#8430=CARTESIAN_POINT('Ctrl Pts',(-0.946873850914351,3.23042227399561,0.457473966449741));
#8431=CARTESIAN_POINT('Ctrl Pts',(-1.05249407916205,3.3024186749887,0.00351263177645307));
#8432=CARTESIAN_POINT('Ctrl Pts',(-0.950881505784981,3.37445127017033,-0.451603133534446));
#8433=CARTESIAN_POINT('Ctrl Pts',(-0.662123411549799,3.44647137006206,-0.81766079968186));
#8434=CARTESIAN_POINT('Ctrl Pts',(-0.243599361895897,3.51843039638608,-1.02223134291874));
#8435=CARTESIAN_POINT('Ctrl Pts',(0.221519869149556,3.59028009019258,-1.02522354552454));
#8436=CARTESIAN_POINT('Ctrl Pts',(0.641079480627667,3.66197241810962,-0.826743985088088));
#8437=CARTESIAN_POINT('Ctrl Pts',(0.932305753772203,3.73346042815455,-0.467154572986677));
#8438=CARTESIAN_POINT('Ctrl Pts',(1.03861864013118,3.80469836360394,-0.0182689927929131));
#8439=CARTESIAN_POINT('Ctrl Pts',(0.940131774495132,3.87564133945326,0.430064269101829));
#8440=CARTESIAN_POINT('Ctrl Pts',(0.627502787803768,3.95409130409743,0.830659036467112));
#8441=CARTESIAN_POINT('Ctrl Pts',(0.102830685831636,4.03984100530226,1.04268581584403));
#8442=CARTESIAN_POINT('Ctrl Pts',(-0.49583525761956,4.13261541880481,0.912068995906106));
#8443=CARTESIAN_POINT('Ctrl Pts',(-0.878366090562576,4.21687097129819,0.508686580065169));
#8444=CARTESIAN_POINT('Ctrl Pts',(-0.992885546867205,4.29278745506574,0.0303715986090578));
#8445=CARTESIAN_POINT('Ctrl Pts',(-0.900857732990206,4.36055726365513,-0.398358938076031));
#8446=CARTESIAN_POINT('Ctrl Pts',(-0.634099084538523,4.42774028194511,-0.742056089518087));
#8447=CARTESIAN_POINT('Ctrl Pts',(-0.291218725591637,4.48691789775377,-0.912954776843569));
#8448=CARTESIAN_POINT('Ctrl Pts',(0.0353338389981778,4.53828673655579,-0.941939927553755));
#8449=CARTESIAN_POINT('Ctrl Pts',(0.399935353975762,4.59661294894598,-0.865337605334092));
#8450=CARTESIAN_POINT('Ctrl Pts',(0.776733005244855,4.66879116737576,-0.573932764898443));
#8451=CARTESIAN_POINT('Ctrl Pts',(0.951069874501058,4.75420618445989,-0.0374521233468979));
#8452=CARTESIAN_POINT('Ctrl Pts',(0.795667633690238,4.83839691545189,0.496192145698146));
#8453=CARTESIAN_POINT('Ctrl Pts',(0.37321551266873,4.92135696236781,0.844777150582056));
#8454=CARTESIAN_POINT('Ctrl Pts',(-0.164103030175536,5.00307222290658,0.89459526891222));
#8455=CARTESIAN_POINT('Ctrl Pts',(-0.629072367177604,5.0835808762759,0.637182693614477));
#8456=CARTESIAN_POINT('Ctrl Pts',(-0.865197189154805,5.16284198642629,0.170019140261218));
#8457=CARTESIAN_POINT('Ctrl Pts',(-0.798632160692577,5.24101666855333,-0.341498002751401));
#8458=CARTESIAN_POINT('Ctrl Pts',(-0.460704756527705,5.31784810950332,-0.720915681127745));
#8459=CARTESIAN_POINT('Ctrl Pts',(0.0250637377885678,5.39406441483692,-0.843757665617551));
#8460=CARTESIAN_POINT('Ctrl Pts',(0.392990376745248,5.45271234048302,-0.707685397427104));
#8461=CARTESIAN_POINT('Ctrl Pts',(0.590886086419297,5.49672449031458,-0.519704269941511));
#8462=CARTESIAN_POINT('Ctrl Pts',(0.690089356012577,5.52426320420706,-0.369685469098573));
#8463=CARTESIAN_POINT('Ctrl Pts',(0.749986856847359,5.54988405732148,-0.211693609781653));
#8464=CARTESIAN_POINT('Ctrl Pts',(0.771247480786565,5.5791110781329,-0.0641437187273063));
#8465=CARTESIAN_POINT('Ctrl Pts',(0.767559108577705,5.5895217918739,0.0617789617871054));
#8466=CARTESIAN_POINT('Ctrl Pts',(0.750267438830112,5.59229078540417,0.1793701629056));
#8467=CARTESIAN_POINT('Ctrl Pts',(0.707806638640959,5.59776618035719,0.312188989757919));
#8468=CARTESIAN_POINT('Ctrl Pts',(0.617454783946614,5.60822690750947,0.464239989617154));
#8469=CARTESIAN_POINT('Ctrl Pts',(0.458222505179838,5.61756366364294,0.631003603405752));
#8470=CARTESIAN_POINT('Ctrl Pts',(0.195608798086434,5.63243894035577,0.764899762204783));
#8471=CARTESIAN_POINT('Ctrl Pts',(-0.156734375337364,5.64804714333712,0.771570078046333));
#8472=CARTESIAN_POINT('Ctrl Pts',(-0.476157477378167,5.66481182477952,0.624830251716582));
#8473=CARTESIAN_POINT('Ctrl Pts',(-0.699166641732472,5.68097672133402,0.354063891223433));
#8474=CARTESIAN_POINT('Ctrl Pts',(-0.781809684955192,5.69734721833354,0.0140380494345926));
#8475=CARTESIAN_POINT('Ctrl Pts',(-0.708225911167346,5.71356808697831,-0.327254794077137));
#8476=CARTESIAN_POINT('Ctrl Pts',(-0.493842847323202,5.72979893847812,-0.601910253289176));
#8477=CARTESIAN_POINT('Ctrl Pts',(-0.181803249930931,5.74597891382901,-0.755179002729622));
#8478=CARTESIAN_POINT('Ctrl Pts',(0.165081534768499,5.76212746374758,-0.757603397746925));
#8479=CARTESIAN_POINT('Ctrl Pts',(0.477820093240158,5.77824890979495,-0.608663812994026));
#8480=CARTESIAN_POINT('Ctrl Pts',(0.6578420250033,5.79164639431488,-0.38407899922635));
#8481=CARTESIAN_POINT('Ctrl Pts',(0.73258150965522,5.80236905918813,-0.170643907361132));
#8482=CARTESIAN_POINT('Ctrl Pts',(0.745186517603766,5.80770263705373,-0.0597742556711138));
#8483=CARTESIAN_POINT('Ctrl Pts',(0.7452477302825,5.81039501584596,-0.00271036138976081));
#8484=CARTESIAN_POINT('Ctrl Pts',(0.73637554456597,-0.034905906819044,0.00149822141910957));
#8485=CARTESIAN_POINT('Ctrl Pts',(0.736315065289215,-0.0322457861110944,
0.0578784184156994));
#8486=CARTESIAN_POINT('Ctrl Pts',(0.723855119649765,-0.0269785274444079,
0.167359731425993));
#8487=CARTESIAN_POINT('Ctrl Pts',(0.650028605659854,-0.0163885254876421,
0.37813983377051));
#8488=CARTESIAN_POINT('Ctrl Pts',(0.472321434225028,-0.00316501922295564,
0.599771077878032));
#8489=CARTESIAN_POINT('Ctrl Pts',(0.163871505776916,0.0127358734384148,
0.746643302062296));
#8490=CARTESIAN_POINT('Ctrl Pts',(-0.178020717494399,0.0286528420536995,
0.744244506328574));
#8491=CARTESIAN_POINT('Ctrl Pts',(-0.485310363153547,0.0445873742153369,
0.593274343279024));
#8492=CARTESIAN_POINT('Ctrl Pts',(-0.696321638562055,0.0605616885113584,
0.32292679089595));
#8493=CARTESIAN_POINT('Ctrl Pts',(-0.768671245607247,0.0765142879587451,
-0.0127547002843979));
#8494=CARTESIAN_POINT('Ctrl Pts',(-0.687406440746895,0.0925926786917108,
-0.346990712173085));
#8495=CARTESIAN_POINT('Ctrl Pts',(-0.468335089496597,0.108466807087251,
-0.612908749333903));
#8496=CARTESIAN_POINT('Ctrl Pts',(-0.154680439727662,0.124863290065507,
-0.757028315693898));
#8497=CARTESIAN_POINT('Ctrl Pts',(0.190960702616625,0.140381605561349,-0.750372135885658));
#8498=CARTESIAN_POINT('Ctrl Pts',(0.448402540405941,0.154868135339886,-0.619139543588245));
#8499=CARTESIAN_POINT('Ctrl Pts',(0.604563248996462,0.164038317486862,-0.455526063286282));
#8500=CARTESIAN_POINT('Ctrl Pts',(0.692801505132577,0.174257916716736,-0.30711527132824));
#8501=CARTESIAN_POINT('Ctrl Pts',(0.734793387939577,0.17965293624963,-0.175936136859199));
#8502=CARTESIAN_POINT('Ctrl Pts',(0.751540048894326,0.18236990875335,-0.0613882223735424));
#8503=CARTESIAN_POINT('Ctrl Pts',(0.7551152768952,0.192373536659344,0.0597671766645886));
#8504=CARTESIAN_POINT('Ctrl Pts',(0.734520628825619,0.220811715526587,0.203550786591925));
#8505=CARTESIAN_POINT('Ctrl Pts',(0.675504633847438,0.246103680576316,0.35918132189048));
#8506=CARTESIAN_POINT('Ctrl Pts',(0.578868420457559,0.272865433995542,0.505257411901041));
#8507=CARTESIAN_POINT('Ctrl Pts',(0.412986321050612,0.309852623360966,0.6626116128106));
#8508=CARTESIAN_POINT('Ctrl Pts',(0.143629214933139,0.354778069813508,0.785256875260767));
#8509=CARTESIAN_POINT('Ctrl Pts',(-0.213273382019863,0.410462823966773,
0.776304802181754));
#8510=CARTESIAN_POINT('Ctrl Pts',(-0.481071653546511,0.456621559736576,
0.640150666335757));
#8511=CARTESIAN_POINT('Ctrl Pts',(-0.645049975399408,0.494083274439161,
0.468120126704292));
#8512=CARTESIAN_POINT('Ctrl Pts',(-0.76767337587426,0.531645444367446,0.263243408444397));
#8513=CARTESIAN_POINT('Ctrl Pts',(-0.829576444241297,0.579005270485107,
-0.0369315336590326));
#8514=CARTESIAN_POINT('Ctrl Pts',(-0.739536781921683,0.636409241730255,
-0.397545468780097));
#8515=CARTESIAN_POINT('Ctrl Pts',(-0.499423699394477,0.694450871439599,
-0.686584733496388));
#8516=CARTESIAN_POINT('Ctrl Pts',(-0.154065623971144,0.753129042169855,
-0.844809002082346));
#8517=CARTESIAN_POINT('Ctrl Pts',(0.230043082427793,0.812469714610742,-0.837675208300425));
#8518=CARTESIAN_POINT('Ctrl Pts',(0.57700732934804,0.872482307649582,-0.662854788878878));
#8519=CARTESIAN_POINT('Ctrl Pts',(0.816658385667676,0.933178947324927,-0.35144538547475));
#8520=CARTESIAN_POINT('Ctrl Pts',(0.898620498059416,0.994565696397896,0.0374277419560443));
#8521=CARTESIAN_POINT('Ctrl Pts',(0.802909951920287,1.05664651863009,0.427776015744673));
#8522=CARTESIAN_POINT('Ctrl Pts',(0.544644961661021,1.11942139023705,0.741567536492036));
#8523=CARTESIAN_POINT('Ctrl Pts',(0.171851593218361,1.18288712411337,0.914331873365365));
#8524=CARTESIAN_POINT('Ctrl Pts',(-0.243417621312868,1.24703708395778,0.908422505121099));
#8525=CARTESIAN_POINT('Ctrl Pts',(-0.619017067558737,1.31186124271971,0.721193184700129));
#8526=CARTESIAN_POINT('Ctrl Pts',(-0.879004743729533,1.37734624187562,0.386310675363197));
#8527=CARTESIAN_POINT('Ctrl Pts',(-0.96906803258655,1.44347559484074,-0.0322424359567551));
#8528=CARTESIAN_POINT('Ctrl Pts',(-0.86790031511075,1.51022949541887,-0.452411800402243));
#8529=CARTESIAN_POINT('Ctrl Pts',(-0.592183196027881,1.57758514542425,-0.790265094277825));
#8530=CARTESIAN_POINT('Ctrl Pts',(-0.193888028157913,1.64551645506606,-0.976825784968679));
#8531=CARTESIAN_POINT('Ctrl Pts',(0.249421550450008,1.71399556449574,-0.972363226152577));
#8532=CARTESIAN_POINT('Ctrl Pts',(0.60558237598945,1.77532311066709,-0.796625051039305));
#8533=CARTESIAN_POINT('Ctrl Pts',(0.8371883048312,1.82929951027981,-0.541571674018944));
#8534=CARTESIAN_POINT('Ctrl Pts',(1.00631683477663,1.89125996956894,-0.183892861007664));
#8535=CARTESIAN_POINT('Ctrl Pts',(1.00242998154866,1.96919011817703,0.330561809156308));
#8536=CARTESIAN_POINT('Ctrl Pts',(0.678046985374588,2.05553891375192,0.799182526288706));
#8537=CARTESIAN_POINT('Ctrl Pts',(0.215592871821504,2.13445507623113,1.0171687785436));
#8538=CARTESIAN_POINT('Ctrl Pts',(-0.245755484917588,2.20575860450121,1.01453735558465));
#8539=CARTESIAN_POINT('Ctrl Pts',(-0.662053460345902,2.27730056442067,0.811105927156774));
#8540=CARTESIAN_POINT('Ctrl Pts',(-0.949698082269248,2.34903208294355,0.446555465549961));
#8541=CARTESIAN_POINT('Ctrl Pts',(-1.05120940332528,2.42090642547716,-0.00756626728458379));
#8542=CARTESIAN_POINT('Ctrl Pts',(-0.945694482920606,2.4928757819371,-0.4615554336784));
#8543=CARTESIAN_POINT('Ctrl Pts',(-0.65373309706183,2.5648890385768,-0.824852112339042));
#8544=CARTESIAN_POINT('Ctrl Pts',(-0.186398333660609,2.64490897695139,-1.04896208339846));
#8545=CARTESIAN_POINT('Ctrl Pts',(0.392428601415204,2.7328524366949,-1.00457390440015));
#8546=CARTESIAN_POINT('Ctrl Pts',(0.885991466423781,2.82859190723886,-0.609209043800457));
#8547=CARTESIAN_POINT('Ctrl Pts',(1.05529995356455,2.91605815749467,-0.0574670440883165));
#8548=CARTESIAN_POINT('Ctrl Pts',(0.9404267219597,2.99525759198824,0.442525460783353));
#8549=CARTESIAN_POINT('Ctrl Pts',(0.654351201989198,3.06625247050285,0.801954035756638));
#8550=CARTESIAN_POINT('Ctrl Pts',(0.242213795090643,3.13691829410408,1.0008916007729));
#8551=CARTESIAN_POINT('Ctrl Pts',(-0.212826652864091,3.20721313967166,1.0015903788085));
#8552=CARTESIAN_POINT('Ctrl Pts',(-0.620911802020433,3.27709644689386,0.806151274826951));
#8553=CARTESIAN_POINT('Ctrl Pts',(-0.902125441555246,3.346530047767,0.455442957406053));
#8554=CARTESIAN_POINT('Ctrl Pts',(-1.00288290378015,3.4154781217763,0.0205687076323444));
#8555=CARTESIAN_POINT('Ctrl Pts',(-0.905954016002294,3.48390687931578,-0.411728459241468));
#8556=CARTESIAN_POINT('Ctrl Pts',(-0.633471988666003,3.55178531279618,-0.756523888501645));
#8557=CARTESIAN_POINT('Ctrl Pts',(-0.241848429631614,3.61908513776168,-0.947526609455785));
#8558=CARTESIAN_POINT('Ctrl Pts',(0.189945078096326,3.68578091114585,-0.949941774132402));
#8559=CARTESIAN_POINT('Ctrl Pts',(0.576477351023386,3.75184999351971,-0.766702857245504));
#8560=CARTESIAN_POINT('Ctrl Pts',(0.842763477392158,3.8172729927887,-0.437388143078907));
#8561=CARTESIAN_POINT('Ctrl Pts',(0.939109365943567,3.8820336930257,-0.0292161955326936));
#8562=CARTESIAN_POINT('Ctrl Pts',(0.849864816244772,3.94611895345907,0.375744052309441));
#8563=CARTESIAN_POINT('Ctrl Pts',(0.568855507252894,4.01656349980271,0.735302720458443));
#8564=CARTESIAN_POINT('Ctrl Pts',(0.100527017909476,4.09306752580417,0.923988313796093));
#8565=CARTESIAN_POINT('Ctrl Pts',(-0.429947676508057,4.17529113638153,0.807712312565125));
#8566=CARTESIAN_POINT('Ctrl Pts',(-0.766751457693363,4.24953574058285,0.451988417955662));
#8567=CARTESIAN_POINT('Ctrl Pts',(-0.867055620215192,4.31614550668835,0.0322747096910515));
#8568=CARTESIAN_POINT('Ctrl Pts',(-0.786433787248155,4.37542306155643,-0.342717095306736));
#8569=CARTESIAN_POINT('Ctrl Pts',(-0.553591509894623,4.43404220613309,-0.642541415975661));
#8570=CARTESIAN_POINT('Ctrl Pts',(-0.254949703661647,4.48557926548469,-0.791315045323506));
#8571=CARTESIAN_POINT('Ctrl Pts',(0.0291570293227571,4.53027084332476,-0.816516772993576));
#8572=CARTESIAN_POINT('Ctrl Pts',(0.34619385996304,4.58098898265564,-0.74988353629077));
#8573=CARTESIAN_POINT('Ctrl Pts',(0.673732054403288,4.64373218633335,-0.496576750812237));
#8574=CARTESIAN_POINT('Ctrl Pts',(0.82549313959929,4.71804398143699,-0.0298835092300268));
#8575=CARTESIAN_POINT('Ctrl Pts',(0.690193167473631,4.79144721668186,0.435414793532684));
#8576=CARTESIAN_POINT('Ctrl Pts',(0.320794878503593,4.86403017533548,0.740603743058106));
#8577=CARTESIAN_POINT('Ctrl Pts',(-0.151524491360473,4.9358681380332,0.784763307633389));
#8578=CARTESIAN_POINT('Ctrl Pts',(-0.563015565921111,5.00708900174122,0.557523867207184));
#8579=CARTESIAN_POINT('Ctrl Pts',(-0.773979622003058,5.0777175836591,0.141392160563352));
#8580=CARTESIAN_POINT('Ctrl Pts',(-0.714701089250428,5.14803770018125,-0.318452831272274));
#8581=CARTESIAN_POINT('Ctrl Pts',(-0.408547263645104,5.21774614874156,-0.663787058404696));
#8582=CARTESIAN_POINT('Ctrl Pts',(0.0377467936430655,5.28789319353309,-0.776707496152719));
#8583=CARTESIAN_POINT('Ctrl Pts',(0.379199506697345,5.3421227793977,-0.652201607333827));
#8584=CARTESIAN_POINT('Ctrl Pts',(0.566192011320162,5.38383905564062,-0.473845537381084));
#8585=CARTESIAN_POINT('Ctrl Pts',(0.657798720524143,5.40903749727977,-0.33633854004436));
#8586=CARTESIAN_POINT('Ctrl Pts',(0.717053599435862,5.43460550016389,-0.179948423725179));
#8587=CARTESIAN_POINT('Ctrl Pts',(0.736001368409038,5.46142838699592,-0.0436390822672414));
#8588=CARTESIAN_POINT('Ctrl Pts',(0.732699533805117,5.47025673802722,0.0641384327733226));
#8589=CARTESIAN_POINT('Ctrl Pts',(0.717267567487411,5.4729425292515,0.172968061121252));
#8590=CARTESIAN_POINT('Ctrl Pts',(0.674294164528167,5.47835838582523,0.306417150876912));
#8591=CARTESIAN_POINT('Ctrl Pts',(0.589367588858167,5.48826679742246,0.448845634849525));
#8592=CARTESIAN_POINT('Ctrl Pts',(0.435863681849203,5.49726231481398,0.610050170577536));
#8593=CARTESIAN_POINT('Ctrl Pts',(0.183474856261557,5.51156216531003,0.738484171703071));
#8594=CARTESIAN_POINT('Ctrl Pts',(-0.15694360185226,5.5266426310904,0.745339088711981));
#8595=CARTESIAN_POINT('Ctrl Pts',(-0.466506518539338,5.54288563637211,0.603119649458923));
#8596=CARTESIAN_POINT('Ctrl Pts',(-0.683508500038263,5.55860912503815,0.339956939095868));
#8597=CARTESIAN_POINT('Ctrl Pts',(-0.76427454408521,5.57458525070198,0.00814296699892715));
#8598=CARTESIAN_POINT('Ctrl Pts',(-0.692356403067418,5.59047260948722,-0.326097245851733));
#8599=CARTESIAN_POINT('Ctrl Pts',(-0.481746476318328,5.60642757350697,-0.596113095643866));
#8600=CARTESIAN_POINT('Ctrl Pts',(-0.17408149905981,5.62238535008145,-0.747388705979419));
#8601=CARTESIAN_POINT('Ctrl Pts',(0.169257356596068,5.63837052884417,-0.749914108394102));
#8602=CARTESIAN_POINT('Ctrl Pts',(0.479957957880237,5.65438561617626,-0.602089252884573));
#8603=CARTESIAN_POINT('Ctrl Pts',(0.659507649463215,5.66774084121688,-0.378313552937684));
#8604=CARTESIAN_POINT('Ctrl Pts',(0.734262801294851,5.67846120191509,-0.164945117362021));
#8605=CARTESIAN_POINT('Ctrl Pts',(0.746897136391519,5.68380075014365,-0.0539621818883113));
#8606=CARTESIAN_POINT('Ctrl Pts',(0.746958383329741,5.68649463580539,0.00313364989116945));
#8607=CARTESIAN_POINT('Ctrl Pts',(0.815814566835808,-0.130330224170313,
0.00608572964042181));
#8608=CARTESIAN_POINT('Ctrl Pts',(0.81574777595044,-0.127392493648317,0.0683497558772952));
#8609=CARTESIAN_POINT('Ctrl Pts',(0.801917574530648,-0.121541016479789,
0.189982180475291));
#8610=CARTESIAN_POINT('Ctrl Pts',(0.720076179708318,-0.109802135369318,
0.423637133286657));
#8611=CARTESIAN_POINT('Ctrl Pts',(0.52257246527071,-0.0950959479830286,
0.670216682430069));
#8612=CARTESIAN_POINT('Ctrl Pts',(0.178979683579792,-0.0773850759889481,
0.833857879295006));
#8613=CARTESIAN_POINT('Ctrl Pts',(-0.202796111060343,-0.0596110875399413,
0.831300817004344));
#8614=CARTESIAN_POINT('Ctrl Pts',(-0.546704079234265,-0.0417815048249506,
0.662418911525214));
#8615=CARTESIAN_POINT('Ctrl Pts',(-0.783372055029714,-0.0238709819185979,
0.35933385919972));
#8616=CARTESIAN_POINT('Ctrl Pts',(-0.864753184875197,-0.00594851111055415,
-0.0178353956933698));
#8617=CARTESIAN_POINT('Ctrl Pts',(-0.773334478176264,0.0121517608065129,
-0.394117637746769));
#8618=CARTESIAN_POINT('Ctrl Pts',(-0.526336675575813,0.0300528300152245,
-0.694128101109789));
#8619=CARTESIAN_POINT('Ctrl Pts',(-0.171927989293085,0.0485816853748002,
-0.856967812451655));
#8620=CARTESIAN_POINT('Ctrl Pts',(0.219241892302673,0.0661435690780971,
-0.849629386053875));
#8621=CARTESIAN_POINT('Ctrl Pts',(0.511269538813996,0.0825752908016491,
-0.700651718265711));
#8622=CARTESIAN_POINT('Ctrl Pts',(0.688212742884786,0.0929688824026967,
-0.515482668277123));
#8623=CARTESIAN_POINT('Ctrl Pts',(0.789271830384269,0.104634211773544,-0.345264898065252));
#8624=CARTESIAN_POINT('Ctrl Pts',(0.835840552685706,0.110681117563011,-0.199292500069916));
#8625=CARTESIAN_POINT('Ctrl Pts',(0.855436969693802,0.113747420452251,-0.0672545127801751));
#8626=CARTESIAN_POINT('Ctrl Pts',(0.859596453826075,0.125693134598882,0.0768115217328358));
#8627=CARTESIAN_POINT('Ctrl Pts',(0.835580628255172,0.158478985952571,0.242058833227751));
#8628=CARTESIAN_POINT('Ctrl Pts',(0.769586439779735,0.186651953774656,0.416048967226574));
#8629=CARTESIAN_POINT('Ctrl Pts',(0.658452988538062,0.21754434815504,0.584536130831614));
#8630=CARTESIAN_POINT('Ctrl Pts',(0.469519452725492,0.259607908285106,0.763402550354253));
#8631=CARTESIAN_POINT('Ctrl Pts',(0.160734960161315,0.311184105034643,0.904533612040456));
#8632=CARTESIAN_POINT('Ctrl Pts',(-0.248644367702824,0.375004866555694,
0.893945308130918));
#8633=CARTESIAN_POINT('Ctrl Pts',(-0.556602119263691,0.428104050100634,
0.737655460917103));
#8634=CARTESIAN_POINT('Ctrl Pts',(-0.745182863285185,0.471182200071971,
0.539740059091461));
#8635=CARTESIAN_POINT('Ctrl Pts',(-0.886266592347643,0.514399233249597,
0.304055938312498));
#8636=CARTESIAN_POINT('Ctrl Pts',(-0.957458750454754,0.568882943884272,
-0.0413059341030232));
#8637=CARTESIAN_POINT('Ctrl Pts',(-0.853887718406504,0.634887576404429,
-0.455926605369635));
#8638=CARTESIAN_POINT('Ctrl Pts',(-0.578091030559718,0.701536127276082,
-0.787776294385279));
#8639=CARTESIAN_POINT('Ctrl Pts',(-0.182233203349808,0.768786900212478,
-0.96900716503876));
#8640=CARTESIAN_POINT('Ctrl Pts',(0.256863321069564,0.836623147963356,-0.960702433495544));
#8641=CARTESIAN_POINT('Ctrl Pts',(0.652172274145209,0.905012686367301,-0.761322606502187));
#8642=CARTESIAN_POINT('Ctrl Pts',(0.924097590363894,0.97392627441344,-0.407635822997762));
#8643=CARTESIAN_POINT('Ctrl Pts',(1.01653217168693,1.04332987603216,0.0320590500081477));
#8644=CARTESIAN_POINT('Ctrl Pts',(0.908582814817597,1.11318792879187,0.471232769692432));
#8645=CARTESIAN_POINT('Ctrl Pts',(0.619256634240865,1.18346212175483,0.822317334790882));
#8646=CARTESIAN_POINT('Ctrl Pts',(0.204150883899283,1.25411247134146,1.01435361293424));
#8647=CARTESIAN_POINT('Ctrl Pts',(-0.255335039468057,1.32509717724887,1.00748846785391));
#8648=CARTESIAN_POINT('Ctrl Pts',(-0.668136059212685,1.39637243934443,0.801328514209242));
#8649=CARTESIAN_POINT('Ctrl Pts',(-0.95178292376863,1.46789329716201,0.435379201029196));
#8650=CARTESIAN_POINT('Ctrl Pts',(-1.04908342032033,1.53961364173694,-0.0186107156222253));
#8651=CARTESIAN_POINT('Ctrl Pts',(-0.939782829063175,1.61148644172385,-0.470873215884411));
#8652=CARTESIAN_POINT('Ctrl Pts',(-0.64485528669132,1.68346331508962,-0.831621436646793));
#8653=CARTESIAN_POINT('Ctrl Pts',(-0.222369067997902,1.75549676069967,-1.02904638344089));
#8654=CARTESIAN_POINT('Ctrl Pts',(0.243955251242134,1.82753697804345,-1.02392596074426));
#8655=CARTESIAN_POINT('Ctrl Pts',(0.615426482313246,1.89153843647028,-0.840188966697125));
#8656=CARTESIAN_POINT('Ctrl Pts',(0.855318789869591,1.94747725405015,-0.575802063324271));
#8657=CARTESIAN_POINT('Ctrl Pts',(1.02946598525039,2.01133219243649,-0.207079962486599));
#8658=CARTESIAN_POINT('Ctrl Pts',(1.02461676742319,2.09098355290074,0.318690126147191));
#8659=CARTESIAN_POINT('Ctrl Pts',(0.696030378324876,2.17824032684713,0.791679926775));
#8660=CARTESIAN_POINT('Ctrl Pts',(0.233125707682883,2.25721084766344,1.00931797385436));
#8661=CARTESIAN_POINT('Ctrl Pts',(-0.224626745482788,2.32796519868402,1.00629897457127));
#8662=CARTESIAN_POINT('Ctrl Pts',(-0.6339746836948,2.39835286352834,0.805772864644811));
#8663=CARTESIAN_POINT('Ctrl Pts',(-0.914248320879519,2.46833600847822,0.449890991772054));
#8664=CARTESIAN_POINT('Ctrl Pts',(-1.01204327526433,2.5378754581275,0.0104708032017498));
#8665=CARTESIAN_POINT('Ctrl Pts',(-0.910398591671283,2.60693484615627,-0.425022640350768));
#8666=CARTESIAN_POINT('Ctrl Pts',(-0.632223205978339,2.67548141089082,-0.770545903348306));
#8667=CARTESIAN_POINT('Ctrl Pts',(-0.19077915573745,2.7510331430239,-0.981739247361055));
#8668=CARTESIAN_POINT('Ctrl Pts',(0.350751639619575,2.83332392956361,-0.939388071703264));
#8669=CARTESIAN_POINT('Ctrl Pts',(0.807381113276876,2.92201019365174,-0.572493800660723));
#8670=CARTESIAN_POINT('Ctrl Pts',(0.962046111870681,3.00226828074056,-0.0660538679639963));
#8671=CARTESIAN_POINT('Ctrl Pts',(0.85713814001635,3.07437416292012,0.389020737528709));
#8672=CARTESIAN_POINT('Ctrl Pts',(0.598160067164623,3.13859474978663,0.71396957225712));
#8673=CARTESIAN_POINT('Ctrl Pts',(0.227513112204098,3.20213038395221,0.892582288991036));
#8674=CARTESIAN_POINT('Ctrl Pts',(-0.179271494271356,3.2649741489312,0.892967527550594));
#8675=CARTESIAN_POINT('Ctrl Pts',(-0.542077110569308,3.32712245118683,0.718969078756907));
#8676=CARTESIAN_POINT('Ctrl Pts',(-0.790803776808349,3.38857518661434,0.408461321979562));
#8677=CARTESIAN_POINT('Ctrl Pts',(-0.879425724537882,3.44933557104976,0.0252016951514755));
#8678=CARTESIAN_POINT('Ctrl Pts',(-0.794189164113485,3.50941028939361,-0.354277655648452));
#8679=CARTESIAN_POINT('Ctrl Pts',(-0.55565506297383,3.56880938467294,-0.655921922746495));
#8680=CARTESIAN_POINT('Ctrl Pts',(-0.213823010267795,3.62754617171746,-0.822536668641497));
#8681=CARTESIAN_POINT('Ctrl Pts',(0.162262209172046,3.68563719276518,-0.824574857159711));
#8682=CARTESIAN_POINT('Ctrl Pts',(0.498443927724332,3.74310228788488,-0.665165063005605));
#8683=CARTESIAN_POINT('Ctrl Pts',(0.729881649584937,3.79996423846298,-0.378933927775719));
#8684=CARTESIAN_POINT('Ctrl Pts',(0.813641419711406,3.85624871099306,-0.0241850976803255));
#8685=CARTESIAN_POINT('Ctrl Pts',(0.736071862764344,3.91198415322131,0.328038266669519));
#8686=CARTESIAN_POINT('Ctrl Pts',(0.491395700987951,3.97333733749312,0.641249037607122));
#8687=CARTESIAN_POINT('Ctrl Pts',(0.0825465259422065,4.04013869614394,0.806230684729123));
#8688=CARTESIAN_POINT('Ctrl Pts',(-0.382721908332906,4.11224152784932,0.704620519826417));
#8689=CARTESIAN_POINT('Ctrl Pts',(-0.680039342190835,4.17771585521766,0.391187900565546));
#8690=CARTESIAN_POINT('Ctrl Pts',(-0.76929256937976,4.23681129620248,0.0188477950203028));
#8691=CARTESIAN_POINT('Ctrl Pts',(-0.697572968880325,4.28971140732258,-0.315886341619577));
#8692=CARTESIAN_POINT('Ctrl Pts',(-0.488579496968913,4.34237812445738,-0.585453783834039));
#8693=CARTESIAN_POINT('Ctrl Pts',(-0.218382589504857,4.38902064898335,-0.72035790737469));
#8694=CARTESIAN_POINT('Ctrl Pts',(0.0405292667616248,4.42974503748388,-0.743431301688004));
#8695=CARTESIAN_POINT('Ctrl Pts',(0.331059864144328,4.4762200910532,-0.682509688425359));
#8696=CARTESIAN_POINT('Ctrl Pts',(0.634311856918423,4.53422578801937,-0.448867806825259));
#8697=CARTESIAN_POINT('Ctrl Pts',(0.777308025703065,4.60380885500111,-0.0121266560714404));
#8698=CARTESIAN_POINT('Ctrl Pts',(0.649801734244585,4.67347927181515,0.42983223429034));
#8699=CARTESIAN_POINT('Ctrl Pts',(0.294762018098257,4.74336277150733,0.724467046814928));
#8700=CARTESIAN_POINT('Ctrl Pts',(-0.166668777047864,4.81354665265108,0.76865483122962));
#8701=CARTESIAN_POINT('Ctrl Pts',(-0.575369590459173,4.88419837300077,0.544172082630653));
#8702=CARTESIAN_POINT('Ctrl Pts',(-0.788825555837623,4.95530546670484,0.125518342670985));
#8703=CARTESIAN_POINT('Ctrl Pts',(-0.729195472479747,5.02721825549986,-0.344625717895169));
#8704=CARTESIAN_POINT('Ctrl Pts',(-0.412514652203176,5.0994646437749,-0.703915590092393));
#8705=CARTESIAN_POINT('Ctrl Pts',(0.057341029939602,5.17342777076928,-0.823123346482292));
#8706=CARTESIAN_POINT('Ctrl Pts',(0.421084654129107,5.23099004767544,-0.692290866908447));
#8707=CARTESIAN_POINT('Ctrl Pts',(0.623676583123104,5.27629737843684,-0.498404376340492));
#8708=CARTESIAN_POINT('Ctrl Pts',(0.720981481628271,5.30284883261904,-0.353297733729362));
#8709=CARTESIAN_POINT('Ctrl Pts',(0.787637776164054,5.33179649000212,-0.177295993368771));
#8710=CARTESIAN_POINT('Ctrl Pts',(0.807127765010578,5.36013926255724,-0.0325341715478286));
#8711=CARTESIAN_POINT('Ctrl Pts',(0.803717919008967,5.36886383773889,0.0748374563281189));
#8712=CARTESIAN_POINT('Ctrl Pts',(0.787724000780127,5.37183929103461,0.19119417816538));
#8713=CARTESIAN_POINT('Ctrl Pts',(0.738463599385226,5.37794236856336,0.343374624218365));
#8714=CARTESIAN_POINT('Ctrl Pts',(0.646480275048873,5.38873716881267,0.497186329070444));
#8715=CARTESIAN_POINT('Ctrl Pts',(0.476828824598579,5.39867186989845,0.675729029825157));
#8716=CARTESIAN_POINT('Ctrl Pts',(0.198605891064882,5.41443508721909,0.817066245403871));
#8717=CARTESIAN_POINT('Ctrl Pts',(-0.178053658883927,5.43111443103978,0.82498012601868));
#8718=CARTESIAN_POINT('Ctrl Pts',(-0.521325053956367,5.44911795950504,0.667232269677396));
#8719=CARTESIAN_POINT('Ctrl Pts',(-0.762617030947825,5.46659296431868,0.374829013448801));
#8720=CARTESIAN_POINT('Ctrl Pts',(-0.852682993465006,5.48438716420124,0.0051664039567747));
#8721=CARTESIAN_POINT('Ctrl Pts',(-0.772478321394041,5.50212402713907,-0.368037589934981));
#8722=CARTESIAN_POINT('Ctrl Pts',(-0.53691097226924,5.51997297991181,-0.670213240800697));
#8723=CARTESIAN_POINT('Ctrl Pts',(-0.191971900623107,5.53786425392876,-0.839929874217262));
#8724=CARTESIAN_POINT('Ctrl Pts',(0.193776022104325,5.55582403655017,-0.842829210365558));
#8725=CARTESIAN_POINT('Ctrl Pts',(0.543544715262778,5.57384759260338,-0.676571074022088));
#8726=CARTESIAN_POINT('Ctrl Pts',(0.746106384594806,5.58891491884207,-0.42410215662072));
#8727=CARTESIAN_POINT('Ctrl Pts',(0.830496541827838,5.6010112007023,-0.183345707690691));
#8728=CARTESIAN_POINT('Ctrl Pts',(0.844806303424896,5.6070611048039,-0.057592728256197));
#8729=CARTESIAN_POINT('Ctrl Pts',(0.844875199123982,5.61009141360481,0.00663345773004059));
#8730=CARTESIAN_POINT('Ctrl Pts',(0.939906438417177,-0.1271841600964,0.00607040646680462));
#8731=CARTESIAN_POINT('Ctrl Pts',(0.939829905991479,-0.123817957632468,
0.0774157245494413));
#8732=CARTESIAN_POINT('Ctrl Pts',(0.923862944900474,-0.117061851724138,
0.2178540076698));
#8733=CARTESIAN_POINT('Ctrl Pts',(0.829693062436053,-0.103560783790796,
0.486577094486074));
#8734=CARTESIAN_POINT('Ctrl Pts',(0.602353829492948,-0.0866284912452825,
0.770507164773516));
#8735=CARTESIAN_POINT('Ctrl Pts',(0.207228405429457,-0.066265606401215,
0.958572222843141));
#8736=CARTESIAN_POINT('Ctrl Pts',(-0.231538164597868,-0.0458367855266242,
0.955647011326686));
#8737=CARTESIAN_POINT('Ctrl Pts',(-0.626436292584032,-0.0253639739002074,
0.761654157498351));
#8738=CARTESIAN_POINT('Ctrl Pts',(-0.897962831308357,-0.00481390438675121,
0.413879414597793));
#8739=CARTESIAN_POINT('Ctrl Pts',(-0.991209135863084,0.0157318195341482,
-0.0185163756664182));
#8740=CARTESIAN_POINT('Ctrl Pts',(-0.886474071362816,0.0364604191400236,
-0.449488692149847));
#8741=CARTESIAN_POINT('Ctrl Pts',(-0.603794204103174,0.0569431903993012,
-0.792698688855432));
#8742=CARTESIAN_POINT('Ctrl Pts',(-0.198747795523654,0.078114638256149,
-0.978858885997804));
#8743=CARTESIAN_POINT('Ctrl Pts',(0.2479569333992,0.098169044818479,-0.970301533460238));
#8744=CARTESIAN_POINT('Ctrl Pts',(0.580826896807821,0.1168969127321,-0.800635303947481));
#8745=CARTESIAN_POINT('Ctrl Pts',(0.782783543487387,0.128755908416602,-0.589061191580284));
#8746=CARTESIAN_POINT('Ctrl Pts',(0.897005783332951,0.141975590455534,-0.396941572724955));
#8747=CARTESIAN_POINT('Ctrl Pts',(0.951220623434889,0.148949509586055,-0.227497964180474));
#8748=CARTESIAN_POINT('Ctrl Pts',(0.972956057301772,0.15245056068407,-0.0791516212742408));
#8749=CARTESIAN_POINT('Ctrl Pts',(0.97754652886228,0.165473006281797,0.0782497587389625));
#8750=CARTESIAN_POINT('Ctrl Pts',(0.951074314734696,0.202035990104472,0.26289373696168));
#8751=CARTESIAN_POINT('Ctrl Pts',(0.875117674322805,0.234575379297086,0.463185600964872));
#8752=CARTESIAN_POINT('Ctrl Pts',(0.750919585816,0.268975213515426,0.650931093138003));
#8753=CARTESIAN_POINT('Ctrl Pts',(0.537696047856619,0.316509625068173,0.85315710508312));
#8754=CARTESIAN_POINT('Ctrl Pts',(0.192140410745468,0.374131477487151,1.01037624365697));
#8755=CARTESIAN_POINT('Ctrl Pts',(-0.264206380811682,0.445324770140323,
0.998717987200337));
#8756=CARTESIAN_POINT('Ctrl Pts',(-0.60497909247259,0.504068055142493,0.825204449287501));
#8757=CARTESIAN_POINT('Ctrl Pts',(-0.812831910323995,0.551561950105494,
0.60706127738152));
#8758=CARTESIAN_POINT('Ctrl Pts',(-0.967790000134998,0.599037654222494,
0.348058819341403));
#8759=CARTESIAN_POINT('Ctrl Pts',(-1.04533263645627,0.6585892857431,-0.0295136425529551));
#8760=CARTESIAN_POINT('Ctrl Pts',(-0.932535340945042,0.730244323598823,
-0.479582476332701));
#8761=CARTESIAN_POINT('Ctrl Pts',(-0.635006531939138,0.802063290813462,
-0.836967292035285));
#8762=CARTESIAN_POINT('Ctrl Pts',(-0.211384495481914,0.873997036925785,
-1.03048411286453));
#8763=CARTESIAN_POINT('Ctrl Pts',(0.254709981643081,0.945997256786745,-1.02125718526525));
#8764=CARTESIAN_POINT('Ctrl Pts',(0.67084303194271,1.01801469476201,-0.810910636057396));
#8765=CARTESIAN_POINT('Ctrl Pts',(0.954585138228141,1.0900005002384,-0.441157482208363));
#8766=CARTESIAN_POINT('Ctrl Pts',(1.04994123186901,1.16190629013951,0.0145248993214667));
#8767=CARTESIAN_POINT('Ctrl Pts',(0.938591683824628,1.23368378508775,0.465709565102106));
#8768=CARTESIAN_POINT('Ctrl Pts',(0.643431339510734,1.30528535077411,0.823184446043401));
#8769=CARTESIAN_POINT('Ctrl Pts',(0.223814954443136,1.37666442496449,1.01682287715933));
#8770=CARTESIAN_POINT('Ctrl Pts',(-0.236531974525708,1.44777562939584,1.00950493693116));
#8771=CARTESIAN_POINT('Ctrl Pts',(-0.646421566503835,1.51857451620532,0.804309277608774));
#8772=CARTESIAN_POINT('Ctrl Pts',(-0.925483599505392,1.58901842308451,0.443565715500478));
#8773=CARTESIAN_POINT('Ctrl Pts',(-1.02010539289345,1.65906655902036,2.42297128055727E-5));
#8774=CARTESIAN_POINT('Ctrl Pts',(-0.913819996698292,1.7286798097062,-0.437968138571777));
#8775=CARTESIAN_POINT('Ctrl Pts',(-0.630160568699183,1.79782128167042,-0.784279189982178));
#8776=CARTESIAN_POINT('Ctrl Pts',(-0.227395315121979,1.86645611005081,-0.972046706488162));
#8777=CARTESIAN_POINT('Ctrl Pts',(0.213444128321082,1.93455302367051,-0.966813468380816));
#8778=CARTESIAN_POINT('Ctrl Pts',(0.561716935446795,1.99457711577682,-0.794168385956479));
#8779=CARTESIAN_POINT('Ctrl Pts',(0.78522515015619,2.04671554814781,-0.547659082460407));
#8780=CARTESIAN_POINT('Ctrl Pts',(0.94663695478074,2.10594250251885,-0.205550399857325));
#8781=CARTESIAN_POINT('Ctrl Pts',(0.941481597089603,2.17927874983002,0.278554385535095));
#8782=CARTESIAN_POINT('Ctrl Pts',(0.641108833826435,2.25889087391522,0.709714880954011));
#8783=CARTESIAN_POINT('Ctrl Pts',(0.221833195347442,2.33039331777189,0.906449037898222));
#8784=CARTESIAN_POINT('Ctrl Pts',(-0.190123342571746,2.39406365797347,0.90345723681407));
#8785=CARTESIAN_POINT('Ctrl Pts',(-0.556303094398879,2.45704563273878,0.723775657346073));
#8786=CARTESIAN_POINT('Ctrl Pts',(-0.805584086874686,2.51933428903179,0.406858637485983));
#8787=CARTESIAN_POINT('Ctrl Pts',(-0.89199844425266,2.58092908865271,0.017575706225503));
#8788=CARTESIAN_POINT('Ctrl Pts',(-0.802166177424502,2.64183226097443,-0.366450158389341));
#8789=CARTESIAN_POINT('Ctrl Pts',(-0.557654608477566,2.70205037551361,-0.669898112087391));
#8790=CARTESIAN_POINT('Ctrl Pts',(-0.171033852000111,2.76820620838145,-0.854685840107926));
#8791=CARTESIAN_POINT('Ctrl Pts',(0.301618002943444,2.84003274926916,-0.817487415729384));
#8792=CARTESIAN_POINT('Ctrl Pts',(0.699057776995513,2.9172448186525,-0.49794966221246));
#8793=CARTESIAN_POINT('Ctrl Pts',(0.833467046929173,2.98702269611,-0.0576334810784838));
#8794=CARTESIAN_POINT('Ctrl Pts',(0.742277817555522,3.04970582955709,0.337953463887036));
#8795=CARTESIAN_POINT('Ctrl Pts',(0.517042943018354,3.10556662329371,0.620609779563879));
#8796=CARTESIAN_POINT('Ctrl Pts',(0.19426341821801,3.16090466964743,0.776222465328461));
#8797=CARTESIAN_POINT('Ctrl Pts',(-0.160746636221079,3.21575319576163,0.776648631182202));
#8798=CARTESIAN_POINT('Ctrl Pts',(-0.478318938585645,3.27014817460386,0.624475708033388));
#8799=CARTESIAN_POINT('Ctrl Pts',(-0.696896151511846,3.324127586389,0.351843616381397));
#8800=CARTESIAN_POINT('Ctrl Pts',(-0.775245270789157,3.37773119830916,0.0137962455995873));
#8801=CARTESIAN_POINT('Ctrl Pts',(-0.699871463303963,3.43100107805136,-0.322711084842332));
#8802=CARTESIAN_POINT('Ctrl Pts',(-0.487321527970625,3.48398070238957,-0.591872409021712));
#8803=CARTESIAN_POINT('Ctrl Pts',(-0.180570652930958,3.53671489691997,-0.741676361489922));
#8804=CARTESIAN_POINT('Ctrl Pts',(0.159499801668676,3.58924970548576,-0.743804151110084));
#8805=CARTESIAN_POINT('Ctrl Pts',(0.466042924677468,3.64163244121242,-0.598790110718948));
#8806=CARTESIAN_POINT('Ctrl Pts',(0.679048172164124,3.69391101203407,-0.335874179181561));
#8807=CARTESIAN_POINT('Ctrl Pts',(0.757098987300611,3.74613352942541,-0.00685566915496274));
#8808=CARTESIAN_POINT('Ctrl Pts',(0.684780334607884,3.79834928453026,0.323157073681087));
#8809=CARTESIAN_POINT('Ctrl Pts',(0.453629101282779,3.85641345347746,0.619779787434268));
#8810=CARTESIAN_POINT('Ctrl Pts',(0.0623550725553726,3.92040805691949,0.778615434185862));
#8811=CARTESIAN_POINT('Ctrl Pts',(-0.390074273721578,3.99049207085899,0.680884262897895));
#8812=CARTESIAN_POINT('Ctrl Pts',(-0.684040858644726,4.05508469998422,0.372336294124342));
#8813=CARTESIAN_POINT('Ctrl Pts',(-0.773782047272804,4.11416918249667,0.000206877778816241));
#8814=CARTESIAN_POINT('Ctrl Pts',(-0.70167834245794,4.16766962919652,-0.338346375873826));
#8815=CARTESIAN_POINT('Ctrl Pts',(-0.488341635818142,4.2215297999684,-0.614253066244098));
#8816=CARTESIAN_POINT('Ctrl Pts',(-0.209132227965426,4.26976699194909,-0.754096345125804));
#8817=CARTESIAN_POINT('Ctrl Pts',(0.0609805405658866,4.31225648238685,-0.77830614316397));
#8818=CARTESIAN_POINT('Ctrl Pts',(0.366234247622769,4.36109387197713,-0.714482850537072));
#8819=CARTESIAN_POINT('Ctrl Pts',(0.688676175467285,4.42268467081582,-0.467077355584903));
#8820=CARTESIAN_POINT('Ctrl Pts',(0.843413801971236,4.49754516558418,0.00243899912125815));
#8821=CARTESIAN_POINT('Ctrl Pts',(0.705411783279281,4.57342125554201,0.483965394365443));
#8822=CARTESIAN_POINT('Ctrl Pts',(0.314963646473482,4.65038440706278,0.809051886098812));
#8823=CARTESIAN_POINT('Ctrl Pts',(-0.198237492464167,4.72846069412574,0.858942600748725));
#8824=CARTESIAN_POINT('Ctrl Pts',(-0.657185748993143,4.80774756578419,0.607608797061368));
#8825=CARTESIAN_POINT('Ctrl Pts',(-0.899024919928932,4.88814942720442,0.134508754564314));
#8826=CARTESIAN_POINT('Ctrl Pts',(-0.831643421949731,4.96996756169197,-0.40042897985535));
#8827=CARTESIAN_POINT('Ctrl Pts',(-0.46987321377987,5.05256463965024,-0.811382428255479));
#8828=CARTESIAN_POINT('Ctrl Pts',(0.0690581953111297,5.1374089989059,-0.948414578263101));
#8829=CARTESIAN_POINT('Ctrl Pts',(0.487312195028491,5.20360536084171,-0.798018478839387));
#8830=CARTESIAN_POINT('Ctrl Pts',(0.720297973143596,5.25569818779602,-0.57510729034124));
#8831=CARTESIAN_POINT('Ctrl Pts',(0.832335357294807,5.28628902729891,-0.407959995971762));
#8832=CARTESIAN_POINT('Ctrl Pts',(0.908873130351851,5.31950870716802,-0.205878602913977));
#8833=CARTESIAN_POINT('Ctrl Pts',(0.931363540892335,5.35216146376384,-0.0392745058560254));
#8834=CARTESIAN_POINT('Ctrl Pts',(0.927434195664507,5.36234522228185,0.0857875461811561));
#8835=CARTESIAN_POINT('Ctrl Pts',(0.908875105564033,5.36576783693661,0.220317388486051));
#8836=CARTESIAN_POINT('Ctrl Pts',(0.852286384985471,5.37279307838038,0.395250245876621));
#8837=CARTESIAN_POINT('Ctrl Pts',(0.746062550306667,5.3852497453038,0.572917610790592));
#8838=CARTESIAN_POINT('Ctrl Pts',(0.550528031875155,5.39670172092908,0.77866612250797));
#8839=CARTESIAN_POINT('Ctrl Pts',(0.229815579370894,5.41487269450219,0.941605990938079));
#8840=CARTESIAN_POINT('Ctrl Pts',(-0.204110926197266,5.43408899022989,0.950683299904042));
#8841=CARTESIAN_POINT('Ctrl Pts',(-0.599371245479392,5.45482050028233,0.769034187245812));
#8842=CARTESIAN_POINT('Ctrl Pts',(-0.87702867899364,5.4749305717571,0.432514158981164));
#8843=CARTESIAN_POINT('Ctrl Pts',(-0.980583112087856,5.49539534630079,0.00737562741174088));
#8844=CARTESIAN_POINT('Ctrl Pts',(-0.888377645682189,5.51577904421374,-0.42153230387796));
#8845=CARTESIAN_POINT('Ctrl Pts',(-0.617828895808705,5.53627666571285,-0.76851148836897));
#8846=CARTESIAN_POINT('Ctrl Pts',(-0.222024165532676,5.5568042851676,-0.963242492518997));
#8847=CARTESIAN_POINT('Ctrl Pts',(0.22023538052913,5.57739671760846,-0.966476782276498));
#8848=CARTESIAN_POINT('Ctrl Pts',(0.620798780318651,5.59803503608039,-0.77611093732286));
#8849=CARTESIAN_POINT('Ctrl Pts',(0.85258883077245,5.61528501724234,-0.487001575340435));
#8850=CARTESIAN_POINT('Ctrl Pts',(0.949002234587475,5.62910083396811,-0.212024071906503));
#8851=CARTESIAN_POINT('Ctrl Pts',(0.965390060580142,5.6360317010903,-0.0679575811816029));
#8852=CARTESIAN_POINT('Ctrl Pts',(0.965468448539529,5.63947951751958,0.00511751240862206));
#8853=CARTESIAN_POINT('Ctrl Pts',(1.01541404854081,-0.0286935421156315,
0.00150443648987817));
#8854=CARTESIAN_POINT('Ctrl Pts',(1.0153316720095,-0.0250702924914887,0.0782977665694167));
#8855=CARTESIAN_POINT('Ctrl Pts',(0.998061067965302,-0.01776881642298,0.230061020652479));
#8856=CARTESIAN_POINT('Ctrl Pts',(0.896507970410834,-0.00321644170734523,
0.519681530472795));
#8857=CARTESIAN_POINT('Ctrl Pts',(0.651700399400465,0.0150138989322842,
0.825300432454518));
#8858=CARTESIAN_POINT('Ctrl Pts',(0.227375973227118,0.036878832048787,1.02708251861184));
#8859=CARTESIAN_POINT('Ctrl Pts',(-0.242679375804631,0.0587675112003217,
1.02386206441447));
#8860=CARTESIAN_POINT('Ctrl Pts',(-0.664613500907547,0.0806464126928114,
0.816420272619932));
#8861=CARTESIAN_POINT('Ctrl Pts',(-0.954028936186183,0.102560724404933,
0.445560203245322));
#8862=CARTESIAN_POINT('Ctrl Pts',(-1.05305061430877,0.124415052527098,-0.0143232362366139));
#8863=CARTESIAN_POINT('Ctrl Pts',(-0.941823920774565,0.146408467527581,
-0.471556911983546));
#8864=CARTESIAN_POINT('Ctrl Pts',(-0.642485376190151,0.168092546430336,
-0.834629545979693));
#8865=CARTESIAN_POINT('Ctrl Pts',(-0.214891649867034,0.190440095097436,
-1.03118613926827));
#8866=CARTESIAN_POINT('Ctrl Pts',(0.255634621569918,0.211565709991131,-1.02177602841285));
#8867=CARTESIAN_POINT('Ctrl Pts',(0.604967188378009,0.231223905635136,-0.843971173664312));
#8868=CARTESIAN_POINT('Ctrl Pts',(0.817375614875641,0.243692331658102,-0.620966234628241));
#8869=CARTESIAN_POINT('Ctrl Pts',(0.93521991933766,0.257410231695498,-0.423284374065397));
#8870=CARTESIAN_POINT('Ctrl Pts',(0.994404452315675,0.264894384309915,-0.239303687432268));
#8871=CARTESIAN_POINT('Ctrl Pts',(1.01596215324894,0.268591201966757,-0.0880723640353921));
#8872=CARTESIAN_POINT('Ctrl Pts',(1.0205039746406,0.281019326474854,0.0630908513062379));
#8873=CARTESIAN_POINT('Ctrl Pts',(0.994378414321425,0.317957096714928,0.250530420627939));
#8874=CARTESIAN_POINT('Ctrl Pts',(0.912951430370462,0.353072056425804,0.465323791815171));
#8875=CARTESIAN_POINT('Ctrl Pts',(0.786921615932354,0.38772781696553,0.654734433319484));
#8876=CARTESIAN_POINT('Ctrl Pts',(0.566396891602532,0.437024433912912,0.864633138859578));
#8877=CARTESIAN_POINT('Ctrl Pts',(0.214287136160365,0.495563811300856,1.02349076931142));
#8878=CARTESIAN_POINT('Ctrl Pts',(-0.248413771213054,0.567872730344711,
1.01212656684935));
#8879=CARTESIAN_POINT('Ctrl Pts',(-0.590158481993694,0.626768703811191,
0.837169097794829));
#8880=CARTESIAN_POINT('Ctrl Pts',(-0.797510277958299,0.674174341970158,
0.619616869419747));
#8881=CARTESIAN_POINT('Ctrl Pts',(-0.951354574490064,0.721326912001104,
0.36226182871036));
#8882=CARTESIAN_POINT('Ctrl Pts',(-1.02758183833276,0.780135727695703,-0.0105470253631208));
#8883=CARTESIAN_POINT('Ctrl Pts',(-0.916742267762083,0.850265458962013,
-0.450941013164969));
#8884=CARTESIAN_POINT('Ctrl Pts',(-0.627617874156891,0.919998168879143,
-0.79759899354444));
#8885=CARTESIAN_POINT('Ctrl Pts',(-0.219645029295957,0.989251615618451,
-0.983505765471186));
#8886=CARTESIAN_POINT('Ctrl Pts',(0.225381885584275,1.05801068462552,-0.974300058686517));
#8887=CARTESIAN_POINT('Ctrl Pts',(0.619361047095629,1.12623348932208,-0.774713667806041));
#8888=CARTESIAN_POINT('Ctrl Pts',(0.885716095501334,1.19389398672781,-0.426999836263685));
#8889=CARTESIAN_POINT('Ctrl Pts',(0.974291026212976,1.26096321722367,-0.00195020977515301));
#8890=CARTESIAN_POINT('Ctrl Pts',(0.870876015266758,1.32741755937141,0.415634325020865));
#8891=CARTESIAN_POINT('Ctrl Pts',(0.599338144996461,1.39323527154609,0.743980912787849));
#8892=CARTESIAN_POINT('Ctrl Pts',(0.216180250636426,1.45839836163331,0.920451353607443));
#8893=CARTESIAN_POINT('Ctrl Pts',(-0.201272117097304,1.52289181314394,0.913522853159369));
#8894=CARTESIAN_POINT('Ctrl Pts',(-0.570548639662344,1.58670389932783,0.728354841003099));
#8895=CARTESIAN_POINT('Ctrl Pts',(-0.820382402521458,1.64982630148298,0.404986062705005));
#8896=CARTESIAN_POINT('Ctrl Pts',(-0.904479685668547,1.71225408373635,0.00968826999415909));
#8897=CARTESIAN_POINT('Ctrl Pts',(-0.810038574444765,1.7739857088511,-0.378630014114413));
#8898=CARTESIAN_POINT('Ctrl Pts',(-0.559509437490529,1.8350230574724,-0.684209923886114));
#8899=CARTESIAN_POINT('Ctrl Pts',(-0.205333854139325,1.89537153055327,-0.849154186548771));
#8900=CARTESIAN_POINT('Ctrl Pts',(0.180913185811132,1.95503963034863,-0.844441083709361));
#8901=CARTESIAN_POINT('Ctrl Pts',(0.485145501820239,2.00748431759449,-0.693529326700443));
#8902=CARTESIAN_POINT('Ctrl Pts',(0.680025653214346,2.05294977689377,-0.4785681353795));
#8903=CARTESIAN_POINT('Ctrl Pts',(0.820569325450077,2.10453041033964,-0.180613181464698));
#8904=CARTESIAN_POINT('Ctrl Pts',(0.816018280899283,2.16830917571319,0.240386482303728));
#8905=CARTESIAN_POINT('Ctrl Pts',(0.554982945114321,2.23749424473742,0.615072637612301));
#8906=CARTESIAN_POINT('Ctrl Pts',(0.190474109677823,2.29966157986966,0.786172683784692));
#8907=CARTESIAN_POINT('Ctrl Pts',(-0.16810567273515,2.35508007174548,0.783641241011412));
#8908=CARTESIAN_POINT('Ctrl Pts',(-0.487480644144325,2.41000246178756,0.627042764779694));
#8909=CARTESIAN_POINT('Ctrl Pts',(-0.705547500524523,2.46446249857771,0.350025298859625));
#8910=CARTESIAN_POINT('Ctrl Pts',(-0.781519650084714,2.51849770387977,0.00853405927247853));
#8911=CARTESIAN_POINT('Ctrl Pts',(-0.702570992198226,2.57214827844602,-0.329827714267465));
#8912=CARTESIAN_POINT('Ctrl Pts',(-0.486274342611164,2.62545312866023,-0.59860543001831));
#8913=CARTESIAN_POINT('Ctrl Pts',(-0.142162838703697,2.68435626813191,-0.763377855466168));
#8914=CARTESIAN_POINT('Ctrl Pts',(0.281841368907173,2.74877887629358,-0.73060196102912));
#8915=CARTESIAN_POINT('Ctrl Pts',(0.642352611343018,2.81872244827704,-0.441705029191515));
#8916=CARTESIAN_POINT('Ctrl Pts',(0.766135230581646,2.88262056243045,-0.0386487887714388));
#8917=CARTESIAN_POINT('Ctrl Pts',(0.682146453828098,2.94061856579323,0.327550649434606));
#8918=CARTESIAN_POINT('Ctrl Pts',(0.471988991973713,2.99280172387605,0.591860756051737));
#8919=CARTESIAN_POINT('Ctrl Pts',(0.167546526079099,3.04501676534233,0.739073495501827));
#8920=CARTESIAN_POINT('Ctrl Pts',(-0.171001703799227,3.09731247177318,0.739884148714911));
#8921=CARTESIAN_POINT('Ctrl Pts',(-0.477304502784758,3.14973690901181,0.593577403675705));
#8922=CARTESIAN_POINT('Ctrl Pts',(-0.690674180169148,3.20233769539631,0.328129045034359));
#8923=CARTESIAN_POINT('Ctrl Pts',(-0.768323012250615,3.25516121598218,-0.00496084478245173));
#8924=CARTESIAN_POINT('Ctrl Pts',(-0.693617521096008,3.30825337771062,-0.340504233555695));
#8925=CARTESIAN_POINT('Ctrl Pts',(-0.479667676648141,3.36165845234506,-0.612152379685385));
#8926=CARTESIAN_POINT('Ctrl Pts',(-0.167078917313426,3.41541915108854,-0.765297478660572));
#8927=CARTESIAN_POINT('Ctrl Pts',(0.183558850259758,3.46957641471836,-0.767927865892618));
#8928=CARTESIAN_POINT('Ctrl Pts',(0.503285298567085,3.52416949866324,-0.617153128637687));
#8929=CARTESIAN_POINT('Ctrl Pts',(0.728015013291304,3.57923520646701,-0.340429122081529));
#8930=CARTESIAN_POINT('Ctrl Pts',(0.811494657084915,3.63480791389034,0.00967126530056645));
#8931=CARTESIAN_POINT('Ctrl Pts',(0.734134654405728,3.69091962908469,0.364469200185399));
#8932=CARTESIAN_POINT('Ctrl Pts',(0.483731297324057,3.75389710925618,0.686496005848039));
#8933=CARTESIAN_POINT('Ctrl Pts',(0.0551920067279564,3.82402651455037,0.861293716109767));
#8934=CARTESIAN_POINT('Ctrl Pts',(-0.446129312901893,3.90164697131953,0.753780321290741));
#8935=CARTESIAN_POINT('Ctrl Pts',(-0.775266770278101,3.97386573112298,0.409205356780351));
#8936=CARTESIAN_POINT('Ctrl Pts',(-0.876587779067353,4.04038539752733,-0.00977508211755218));
#8937=CARTESIAN_POINT('Ctrl Pts',(-0.795163896594075,4.10093301846076,-0.393025295166194));
#8938=CARTESIAN_POINT('Ctrl Pts',(-0.552701413631269,4.16217441976383,-0.706895391311044));
#8939=CARTESIAN_POINT('Ctrl Pts',(-0.234038723763906,4.21722706264337,-0.866632297588611));
#8940=CARTESIAN_POINT('Ctrl Pts',(0.0751068254044917,4.26585255357816,-0.894373061766401));
#8941=CARTESIAN_POINT('Ctrl Pts',(0.42505471576597,4.32183524942327,-0.821248980428701));
#8942=CARTESIAN_POINT('Ctrl Pts',(0.795538664900941,4.39258201646211,-0.53714913283713));
#8943=CARTESIAN_POINT('Ctrl Pts',(0.973592661579039,4.47869159574723,0.00294967027693707));
#8944=CARTESIAN_POINT('Ctrl Pts',(0.814764167968699,4.56598160688673,0.556927408855015));
#8945=CARTESIAN_POINT('Ctrl Pts',(0.365947861529639,4.65442275123741,0.93038704854384));
#8946=CARTESIAN_POINT('Ctrl Pts',(-0.222497764166292,4.74394347109101,0.98733029944098));
#8947=CARTESIAN_POINT('Ctrl Pts',(-0.746767612105839,4.83453546306066,0.69978571984963));
#8948=CARTESIAN_POINT('Ctrl Pts',(-1.02143955519273,4.9260176862291,0.161418306938975));
#8949=CARTESIAN_POINT('Ctrl Pts',(-0.944719913007531,5.01856725062234,-0.443919063426878));
#8950=CARTESIAN_POINT('Ctrl Pts',(-0.537274670503414,5.11151402622739,-0.905277409599477));
#8951=CARTESIAN_POINT('Ctrl Pts',(0.0642159068265587,5.20609904237226,-1.0582150867811));
#8952=CARTESIAN_POINT('Ctrl Pts',(0.528130756131502,5.27971987016299,-0.889732582513035));
#8953=CARTESIAN_POINT('Ctrl Pts',(0.783429970494387,5.33668529254443,-0.646138507796482));
#8954=CARTESIAN_POINT('Ctrl Pts',(0.908143095679349,5.37096072629315,-0.459096780980709));
#8955=CARTESIAN_POINT('Ctrl Pts',(0.989605658092228,5.40613046868718,-0.244086405525751));
#8956=CARTESIAN_POINT('Ctrl Pts',(1.01529199200331,5.44263887842801,-0.0586913908545394));
#8957=CARTESIAN_POINT('Ctrl Pts',(1.01082053212328,5.45474573741654,0.0888385633722979));
#8958=CARTESIAN_POINT('Ctrl Pts',(0.989621265793943,5.45843623062483,0.238512855713079));
#8959=CARTESIAN_POINT('Ctrl Pts',(0.930168823774541,5.46592421796278,0.423104870225524));
#8960=CARTESIAN_POINT('Ctrl Pts',(0.813228983696787,5.4795677442685,0.619152823787792));
#8961=CARTESIAN_POINT('Ctrl Pts',(0.601537180242377,5.49197366268454,0.841509797706045));
#8962=CARTESIAN_POINT('Ctrl Pts',(0.253625678769957,5.51168590377359,1.01850144143581));
#8963=CARTESIAN_POINT('Ctrl Pts',(-0.215557143609538,5.53247096280752,1.02795739263416));
#8964=CARTESIAN_POINT('Ctrl Pts',(-0.642009135344561,5.55484828747929,0.831989439847644));
#8965=CARTESIAN_POINT('Ctrl Pts',(-0.940774441608774,5.57649768588922,0.469624887452474));
#8966=CARTESIAN_POINT('Ctrl Pts',(-1.05185609843952,5.59848042348958,0.0130672783119852));
#8967=CARTESIAN_POINT('Ctrl Pts',(-0.95294724142773,5.6203207553287,-0.446431339614107));
#8968=CARTESIAN_POINT('Ctrl Pts',(-0.663635568817441,5.64223553779152,-0.817195637636098));
#8969=CARTESIAN_POINT('Ctrl Pts',(-0.241597801203389,5.66412201642128,-1.02472095530409));
#8970=CARTESIAN_POINT('Ctrl Pts',(0.228854601267908,5.68603053593709,-1.02797194332589));
#8971=CARTESIAN_POINT('Ctrl Pts',(0.65379320906392,5.70792720813883,-0.825928779568734));
#8972=CARTESIAN_POINT('Ctrl Pts',(0.899104794299161,5.72619390359354,-0.519721925751465));
#8973=CARTESIAN_POINT('Ctrl Pts',(1.00091159660272,5.74078191241576,-0.229396086229819));
#8974=CARTESIAN_POINT('Ctrl Pts',(1.01823042784667,5.74810326039065,-0.0772232183289336));
#8975=CARTESIAN_POINT('Ctrl Pts',(1.01831301276113,5.75173567571447,-0.000235624821140368));
#8976=CARTESIAN_POINT('Ctrl Pts',(0.984648983550121,0.0916287761618602,
-0.00420559214620277));
#8977=CARTESIAN_POINT('Ctrl Pts',(0.984569074047288,0.0951435159976226,
0.070287916264845));
#8978=CARTESIAN_POINT('Ctrl Pts',(0.96785159059107,0.102215071827367,0.217284031811231));
#8979=CARTESIAN_POINT('Ctrl Pts',(0.869509369496233,0.116307240942699,0.497768770660214));
#8980=CARTESIAN_POINT('Ctrl Pts',(0.632970632528384,0.133912282411646,0.792860122220623));
#8981=CARTESIAN_POINT('Ctrl Pts',(0.224010397149195,0.154982246000659,0.987232026634351));
#8982=CARTESIAN_POINT('Ctrl Pts',(-0.227738935737947,0.176014947093011,
0.983956925535199));
#8983=CARTESIAN_POINT('Ctrl Pts',(-0.632225622436782,0.196990217342226,
0.784980269761374));
#8984=CARTESIAN_POINT('Ctrl Pts',(-0.908833156779193,0.217937334695042,
0.430268392775773));
#8985=CARTESIAN_POINT('Ctrl Pts',(-1.00315714269518,0.238779889329383,-0.00839180413288515));
#8986=CARTESIAN_POINT('Ctrl Pts',(-0.897234292107521,0.259696501114417,
-0.443410759159778));
#8987=CARTESIAN_POINT('Ctrl Pts',(-0.613012989293456,0.28027363660682,-0.787843327150621));
#8988=CARTESIAN_POINT('Ctrl Pts',(-0.208321048403559,0.301410715181248,
-0.973943372778342));
#8989=CARTESIAN_POINT('Ctrl Pts',(0.236187823064961,0.321365472013982,-0.96472154867092));
#8990=CARTESIAN_POINT('Ctrl Pts',(0.564934420323231,0.339858954187646,-0.797635836250644));
#8991=CARTESIAN_POINT('Ctrl Pts',(0.765284272143534,0.351610475561473,-0.586892505079194));
#8992=CARTESIAN_POINT('Ctrl Pts',(0.874430977800043,0.364384335814288,-0.404270210132846));
#8993=CARTESIAN_POINT('Ctrl Pts',(0.932132473479406,0.37156393468169,-0.225771771401753));
#8994=CARTESIAN_POINT('Ctrl Pts',(0.951322910554871,0.375063708484045,-0.0873015561040709));
#8995=CARTESIAN_POINT('Ctrl Pts',(0.95537658577755,0.385668685648629,0.042720286905362));
#8996=CARTESIAN_POINT('Ctrl Pts',(0.932151401111379,0.419279012282826,0.21413345826893));
#8997=CARTESIAN_POINT('Ctrl Pts',(0.853913450916173,0.453214817731995,0.420579039328621));
#8998=CARTESIAN_POINT('Ctrl Pts',(0.738712459359737,0.48466333959355,0.592718978656939));
#8999=CARTESIAN_POINT('Ctrl Pts',(0.533467422810344,0.530659406988462,0.788734527193056));
#9000=CARTESIAN_POINT('Ctrl Pts',(0.210148474461089,0.584247998551829,0.933437435420979));
#9001=CARTESIAN_POINT('Ctrl Pts',(-0.213066084232724,0.650471539673848,
0.923488122281593));
#9002=CARTESIAN_POINT('Ctrl Pts',(-0.522860245212984,0.70381943751296,0.764083825730224));
#9003=CARTESIAN_POINT('Ctrl Pts',(-0.710230955483532,0.746670035618981,
0.567563588265933));
#9004=CARTESIAN_POINT('Ctrl Pts',(-0.848761892340287,0.789134351036642,
0.335658385105654));
#9005=CARTESIAN_POINT('Ctrl Pts',(-0.916893515971457,0.841853183525993,
0.00135356844800982));
#9006=CARTESIAN_POINT('Ctrl Pts',(-0.81780076857272,0.904401699226823,-0.391436604244268));
#9007=CARTESIAN_POINT('Ctrl Pts',(-0.561076476779489,0.966259749866032,
-0.698868666319774));
#9008=CARTESIAN_POINT('Ctrl Pts',(-0.200613927988294,1.02742594336109,-0.86292405532288));
#9009=CARTESIAN_POINT('Ctrl Pts',(0.190898801358669,1.08790487580521,-0.854643120270496));
#9010=CARTESIAN_POINT('Ctrl Pts',(0.536220910044881,1.14770382643931,-0.679543997807491));
#9011=CARTESIAN_POINT('Ctrl Pts',(0.768939370840714,1.20683412954839,-0.375539600166186));
#9012=CARTESIAN_POINT('Ctrl Pts',(0.84608550733363,1.26531015149593,-0.00487186504282669));
#9013=CARTESIAN_POINT('Ctrl Pts',(0.755997632036065,1.32314974933626,0.358619972297139));
#9014=CARTESIAN_POINT('Ctrl Pts',(0.51984856794744,1.38037392798047,0.644112483671553));
#9015=CARTESIAN_POINT('Ctrl Pts',(0.186797875670655,1.4370066824962,0.797492861272122));
#9016=CARTESIAN_POINT('Ctrl Pts',(-0.176167084506555,1.49307481265338,0.791485998881262));
#9017=CARTESIAN_POINT('Ctrl Pts',(-0.497595223102844,1.54860817405036,0.630362526553513));
#9018=CARTESIAN_POINT('Ctrl Pts',(-0.715487592961372,1.60363908336117,0.348459189956295));
#9019=CARTESIAN_POINT('Ctrl Pts',(-0.789099563909685,1.65820225483128,0.00294658455629332));
#9020=CARTESIAN_POINT('Ctrl Pts',(-0.706405422251732,1.71233471279791,-0.337633601053105));
#9021=CARTESIAN_POINT('Ctrl Pts',(-0.485930302287288,1.76607595930567,-0.606810242202756));
#9022=CARTESIAN_POINT('Ctrl Pts',(-0.17264525878764,1.81946665376375,-0.752921334364951));
#9023=CARTESIAN_POINT('Ctrl Pts',(0.170998393471184,1.87255006029022,-0.74894300281477));
#9024=CARTESIAN_POINT('Ctrl Pts',(0.443471026407504,1.91950038239868,-0.614029119564585));
#9025=CARTESIAN_POINT('Ctrl Pts',(0.619041287830423,1.96044279001245,-0.420489990106911));
#9026=CARTESIAN_POINT('Ctrl Pts',(0.746324423909596,2.00712483590238,-0.15090641186216));
#9027=CARTESIAN_POINT('Ctrl Pts',(0.742795882826775,2.06530367893983,0.233138381400874));
#9028=CARTESIAN_POINT('Ctrl Pts',(0.502513298903239,2.12915318805118,0.579348112036599));
#9029=CARTESIAN_POINT('Ctrl Pts',(0.16253718014326,2.18716317053762,0.739396339894856));
#9030=CARTESIAN_POINT('Ctrl Pts',(-0.17539831795519,2.23939524780309,0.73736054879534));
#9031=CARTESIAN_POINT('Ctrl Pts',(-0.479690868610869,2.29169807469187,0.588598159081229));
#9032=CARTESIAN_POINT('Ctrl Pts',(-0.689894606425972,2.34412032601839,0.322210826352658));
#9033=CARTESIAN_POINT('Ctrl Pts',(-0.764219381102178,2.39670968207434,-0.0100147764634279));
#9034=CARTESIAN_POINT('Ctrl Pts',(-0.686940088797011,2.44951251931434,-0.343092764626077));
#9035=CARTESIAN_POINT('Ctrl Pts',(-0.471963980624939,2.50257679039761,-0.61087531074171));
#9036=CARTESIAN_POINT('Ctrl Pts',(-0.125846100986523,2.56186866776871,-0.777155895496916));
#9037=CARTESIAN_POINT('Ctrl Pts',(0.306695745076419,2.62758939711501,-0.744675068695687));
#9038=CARTESIAN_POINT('Ctrl Pts',(0.680536925772417,2.69999236610502,-0.44645395946444));
#9039=CARTESIAN_POINT('Ctrl Pts',(0.811399634809351,2.76710302983079,-0.0234435082030726));
#9040=CARTESIAN_POINT('Ctrl Pts',(0.722567452530805,2.82876532932536,0.365948667491797));
#9041=CARTESIAN_POINT('Ctrl Pts',(0.497274836283305,2.88479222540301,0.649896079203092));
#9042=CARTESIAN_POINT('Ctrl Pts',(0.167565378605837,2.94138117554149,0.809752108634447));
#9043=CARTESIAN_POINT('Ctrl Pts',(-0.202514861231675,2.99855915881875,0.810987742795578));
#9044=CARTESIAN_POINT('Ctrl Pts',(-0.54024836777901,3.05635084400284,0.650034647856289));
#9045=CARTESIAN_POINT('Ctrl Pts',(-0.777439808371775,3.11477744451591,0.355437259411251));
#9046=CARTESIAN_POINT('Ctrl Pts',(-0.864538532626252,3.17385708103057,-0.0169620644579516));
#9047=CARTESIAN_POINT('Ctrl Pts',(-0.780730355879149,3.23360478205715,-0.394546823931951));
#9048=CARTESIAN_POINT('Ctrl Pts',(-0.538871430519538,3.29403218226595,-0.701989737522886));
#9049=CARTESIAN_POINT('Ctrl Pts',(-0.183675044177321,3.35514758348308,-0.876223096704092));
#9050=CARTESIAN_POINT('Ctrl Pts',(0.21641742511937,3.41695593657272,-0.879385005360802));
#9051=CARTESIAN_POINT('Ctrl Pts',(0.58244885584365,3.4794588064082,-0.70691401895504));
#9052=CARTESIAN_POINT('Ctrl Pts',(0.840377488385198,3.54265437797189,-0.389457958817879));
#9053=CARTESIAN_POINT('Ctrl Pts',(0.936379051461337,3.60653744708314,0.0129064008869146));
#9054=CARTESIAN_POINT('Ctrl Pts',(0.847406337365262,3.67109977077888,0.421057242306564));
#9055=CARTESIAN_POINT('Ctrl Pts',(0.559284515754883,3.74357723142762,0.791598570275586));
#9056=CARTESIAN_POINT('Ctrl Pts',(0.0664802120480439,3.82422657018271,0.992494006014603));
#9057=CARTESIAN_POINT('Ctrl Pts',(-0.508836939749483,3.91331939878274,0.868903160147672));
#9058=CARTESIAN_POINT('Ctrl Pts',(-0.885220448376754,3.99595408400187,0.474453579430707));
#9059=CARTESIAN_POINT('Ctrl Pts',(-1.00056529854099,4.07180730080897,-0.00329165097347213));
#9060=CARTESIAN_POINT('Ctrl Pts',(-0.907890405064184,4.14060796730828,-0.43868077322946));
#9061=CARTESIAN_POINT('Ctrl Pts',(-0.633413258504046,4.20990094390894,-0.793653263367458));
#9062=CARTESIAN_POINT('Ctrl Pts',(-0.274462526690471,4.27190716068393,-0.973358002930129));
#9063=CARTESIAN_POINT('Ctrl Pts',(0.0721614216821628,4.32643224508216,-1.00438010445284));
#9064=CARTESIAN_POINT('Ctrl Pts',(0.463151416323009,4.38898332141623,-0.922576230659944));
#9065=CARTESIAN_POINT('Ctrl Pts',(0.874381781681704,4.46758260884606,-0.60648434106529));
#9066=CARTESIAN_POINT('Ctrl Pts',(1.06980246797287,4.5624608610176,-0.0111547350400171));
#9067=CARTESIAN_POINT('Ctrl Pts',(0.895542839263134,4.65778864543642,0.593582242631324));
#9068=CARTESIAN_POINT('Ctrl Pts',(0.409432656352506,4.75346464397675,0.996900689499745));
#9069=CARTESIAN_POINT('Ctrl Pts',(-0.220974884955076,4.8493586118428,1.0569724532724));
#9070=CARTESIAN_POINT('Ctrl Pts',(-0.776343503280075,4.94539607569114,0.751232219154683));
#9071=CARTESIAN_POINT('Ctrl Pts',(-1.06353864055222,5.04137406111148,0.186094576072339));
#9072=CARTESIAN_POINT('Ctrl Pts',(-0.983004483323193,5.13736802025292,-0.442038732586129));
#9073=CARTESIAN_POINT('Ctrl Pts',(-0.563899268862914,5.23282576403033,-0.914456728983043));
#9074=CARTESIAN_POINT('Ctrl Pts',(0.0462535987950873,5.32862941387192,-1.06937942849709));
#9075=CARTESIAN_POINT('Ctrl Pts',(0.512328791044282,5.4028182967163,-0.898072195820719));
#9076=CARTESIAN_POINT('Ctrl Pts',(0.764973310859695,5.45905280441918,-0.657803543587761));
#9077=CARTESIAN_POINT('Ctrl Pts',(0.890710367977351,5.49386603690105,-0.468087075222217));
#9078=CARTESIAN_POINT('Ctrl Pts',(0.968409565374987,5.52718349212031,-0.263107453230972));
#9079=CARTESIAN_POINT('Ctrl Pts',(0.995071164043899,5.56417283457121,-0.076219039962342));
#9080=CARTESIAN_POINT('Ctrl Pts',(0.990445839819153,5.57721055288114,0.0815576822316796));
#9081=CARTESIAN_POINT('Ctrl Pts',(0.968532969593368,5.58078474935199,0.231884168081497));
#9082=CARTESIAN_POINT('Ctrl Pts',(0.912864182508467,5.58792083788095,0.405697502925931));
#9083=CARTESIAN_POINT('Ctrl Pts',(0.79685593045897,5.6013750719408,0.600721988903217));
#9084=CARTESIAN_POINT('Ctrl Pts',(0.590987347316022,5.61344502070309,0.816500282778712));
#9085=CARTESIAN_POINT('Ctrl Pts',(0.251816999969086,5.63265781325075,0.989312986130609));
#9086=CARTESIAN_POINT('Ctrl Pts',(-0.203712241550418,5.652836559154,0.998070068603191));
#9087=CARTESIAN_POINT('Ctrl Pts',(-0.61681159855121,5.67451656195012,0.80825617493892));
#9088=CARTESIAN_POINT('Ctrl Pts',(-0.905346760987353,5.69542976164301,0.45798872211099));
#9089=CARTESIAN_POINT('Ctrl Pts',(-1.01228962463618,5.71661306203865,0.017991770284493));
#9090=CARTESIAN_POINT('Ctrl Pts',(-0.917075602975552,5.73760403864021,-0.423685145857852));
#9091=CARTESIAN_POINT('Ctrl Pts',(-0.639635441889197,5.75860936766058,-0.77908140747453));
#9092=CARTESIAN_POINT('Ctrl Pts',(-0.235928437930338,5.77954061301565,-0.977430172367204));
#9093=CARTESIAN_POINT('Ctrl Pts',(0.212816369821538,5.80043496339875,-0.980446947576766));
#9094=CARTESIAN_POINT('Ctrl Pts',(0.617105887642918,5.82126950130601,-0.788055472477775));
#9095=CARTESIAN_POINT('Ctrl Pts',(0.849818947223183,5.83860198442984,-0.49741920984452));
#9096=CARTESIAN_POINT('Ctrl Pts',(0.946233465126923,5.85242411596325,-0.222305253914967));
#9097=CARTESIAN_POINT('Ctrl Pts',(0.962588059762422,5.85934575684304,-0.0784255384345603));
#9098=CARTESIAN_POINT('Ctrl Pts',(0.962666377720516,5.8627904943351,-0.00541570169036758));
#9099=CARTESIAN_POINT('Ctrl Pts',(0.90955220090418,0.125678856736808,-0.00589269379913899));
#9100=CARTESIAN_POINT('Ctrl Pts',(0.909478225648677,0.128932584618482,0.0630687703907631));
#9101=CARTESIAN_POINT('Ctrl Pts',(0.894048295886179,0.135454695280294,0.198633746114812));
#9102=CARTESIAN_POINT('Ctrl Pts',(0.803209936276703,0.148472212309086,0.457715426009415));
#9103=CARTESIAN_POINT('Ctrl Pts',(0.584980168342948,0.164709446618313,0.729811293679696));
#9104=CARTESIAN_POINT('Ctrl Pts',(0.208027170967614,0.184132547183783,0.90896385424324));
#9105=CARTESIAN_POINT('Ctrl Pts',(-0.207959759216391,0.203501125169494,
0.905893140126457));
#9106=CARTESIAN_POINT('Ctrl Pts',(-0.580071872739438,0.222800673169386,
0.722802863656692));
#9107=CARTESIAN_POINT('Ctrl Pts',(-0.834346439551474,0.242061866579171,
0.396677481020101));
#9108=CARTESIAN_POINT('Ctrl Pts',(-0.92094289121704,0.261209977709745,-0.00626201767291697));
#9109=CARTESIAN_POINT('Ctrl Pts',(-0.823680568403855,0.280412428111005,
-0.405548844365146));
#9110=CARTESIAN_POINT('Ctrl Pts',(-0.562944356772313,0.299290170930855,
-0.721426233726792));
#9111=CARTESIAN_POINT('Ctrl Pts',(-0.191976003784791,0.31866955507914,-0.89198669771893));
#9112=CARTESIAN_POINT('Ctrl Pts',(0.215171433213828,0.33694918115194,-0.883456498426514));
#9113=CARTESIAN_POINT('Ctrl Pts',(0.516068099710212,0.35388104972228,-0.730545197447956));
#9114=CARTESIAN_POINT('Ctrl Pts',(0.69948513866957,0.364640684639828,-0.537522963098884));
#9115=CARTESIAN_POINT('Ctrl Pts',(0.799020464603065,0.376306845093206,-0.37106440995685));
#9116=CARTESIAN_POINT('Ctrl Pts',(0.852211021510913,0.382906747014502,-0.206674942188407));
#9117=CARTESIAN_POINT('Ctrl Pts',(0.869552750695885,0.386118378167317,-0.0807135116177633));
#9118=CARTESIAN_POINT('Ctrl Pts',(0.873228226002728,0.395604438926807,0.0358634082412919));
#9119=CARTESIAN_POINT('Ctrl Pts',(0.852178260557866,0.42620902392069,0.192171108460186));
#9120=CARTESIAN_POINT('Ctrl Pts',(0.780192267650991,0.457471749380521,0.382133130394898));
#9121=CARTESIAN_POINT('Ctrl Pts',(0.675189726878795,0.486095153937536,0.538855525199464));
#9122=CARTESIAN_POINT('Ctrl Pts',(0.487448733465738,0.52819382223328,0.718280709852067));
#9123=CARTESIAN_POINT('Ctrl Pts',(0.192301074143443,0.577093945556737,0.850202458087255));
#9124=CARTESIAN_POINT('Ctrl Pts',(-0.194211405236157,0.63760673037774,0.841257470744877));
#9125=CARTESIAN_POINT('Ctrl Pts',(-0.477073537388488,0.686323304344046,
0.695647695880699));
#9126=CARTESIAN_POINT('Ctrl Pts',(-0.648205135382649,0.725464891967771,
0.516199282848472));
#9127=CARTESIAN_POINT('Ctrl Pts',(-0.774761683593055,0.764262912420243,
0.304335592440901));
#9128=CARTESIAN_POINT('Ctrl Pts',(-0.83712527622246,0.812496673215361,-0.00140070915450113));
#9129=CARTESIAN_POINT('Ctrl Pts',(-0.746440875151343,0.869769816513919,
-0.361038867683182));
#9130=CARTESIAN_POINT('Ctrl Pts',(-0.510939112655819,0.926556842886396,
-0.643231430899843));
#9131=CARTESIAN_POINT('Ctrl Pts',(-0.179428142008608,0.982828907729359,
-0.79421329029021));
#9132=CARTESIAN_POINT('Ctrl Pts',(0.18174936978697,1.03863921522632,-0.786712467357663));
#9133=CARTESIAN_POINT('Ctrl Pts',(0.501469893757735,1.09400777439781,-0.624757152462634));
#9134=CARTESIAN_POINT('Ctrl Pts',(0.717864370714667,1.14897277405206,-0.342352558018187));
#9135=CARTESIAN_POINT('Ctrl Pts',(0.790049385509793,1.20356691455005,0.00357612389287991));
#9136=CARTESIAN_POINT('Ctrl Pts',(0.705754196611436,1.25782823693133,0.344532532610256));
#9137=CARTESIAN_POINT('Ctrl Pts',(0.483277370716406,1.31179498215349,0.613838500779083));
#9138=CARTESIAN_POINT('Ctrl Pts',(0.167585716227014,1.3655073441895,0.759481897321007));
#9139=CARTESIAN_POINT('Ctrl Pts',(-0.178658312614736,1.41900638076518,0.754000347388005));
#9140=CARTESIAN_POINT('Ctrl Pts',(-0.487358805469693,1.4723346864654,0.599549639426908));
#9141=CARTESIAN_POINT('Ctrl Pts',(-0.698165752470841,1.52553548174234,0.32725969494298));
#9142=CARTESIAN_POINT('Ctrl Pts',(-0.770084936124923,1.57865238683387,-0.00895031380089644));
#9143=CARTESIAN_POINT('Ctrl Pts',(-0.689303462132877,1.63172997477994,-0.342877489010814));
#9144=CARTESIAN_POINT('Ctrl Pts',(-0.471811562324975,1.68481246545016,-0.60887894620495));
#9145=CARTESIAN_POINT('Ctrl Pts',(-0.160236777931869,1.73794563714968,-0.75451752224437));
#9146=CARTESIAN_POINT('Ctrl Pts',(0.184257032273775,1.79117120239166,-0.750831658503854));
#9147=CARTESIAN_POINT('Ctrl Pts',(0.45962358205835,1.83861061933306,-0.614790911954126));
#9148=CARTESIAN_POINT('Ctrl Pts',(0.638154679941761,1.88022882117527,-0.418143586816256));
#9149=CARTESIAN_POINT('Ctrl Pts',(0.768250650239937,1.92791038289434,-0.142887497408747));
#9150=CARTESIAN_POINT('Ctrl Pts',(0.765210575236715,1.98778313244085,0.252300460533073));
#9151=CARTESIAN_POINT('Ctrl Pts',(0.516123981662164,2.05410503330788,0.6122539442656));
#9152=CARTESIAN_POINT('Ctrl Pts',(0.160263722031045,2.11485118755329,0.780150477387041));
#9153=CARTESIAN_POINT('Ctrl Pts',(-0.195888391503639,2.16990388596071,0.778274632766191));
#9154=CARTESIAN_POINT('Ctrl Pts',(-0.518660047512728,2.22536566924697,0.620779215863372));
#9155=CARTESIAN_POINT('Ctrl Pts',(-0.743027269231705,2.28127313124113,0.336845813371297));
#9156=CARTESIAN_POINT('Ctrl Pts',(-0.822939493772593,2.33765555827195,-0.0192857525782725));
#9157=CARTESIAN_POINT('Ctrl Pts',(-0.739895966613412,2.39454181187788,-0.378174258410101));
#9158=CARTESIAN_POINT('Ctrl Pts',(-0.507432703799843,2.45195821290454,-0.668052190846269));
#9159=CARTESIAN_POINT('Ctrl Pts',(-0.131531364679454,2.51636641537369,-0.848855077071543));
#9160=CARTESIAN_POINT('Ctrl Pts',(0.340198775675162,2.58803340462628,-0.813744118818101));
#9161=CARTESIAN_POINT('Ctrl Pts',(0.749550293417911,2.66727724174046,-0.487526234835778));
#9162=CARTESIAN_POINT('Ctrl Pts',(0.893316574148684,2.74091681990833,-0.023366466522462));
#9163=CARTESIAN_POINT('Ctrl Pts',(0.795757990210055,2.80866966254995,0.404576874166815));
#9164=CARTESIAN_POINT('Ctrl Pts',(0.548004150809532,2.87027962092074,0.716888421623811));
#9165=CARTESIAN_POINT('Ctrl Pts',(0.185289053539309,2.93252341178201,0.892760490208275));
#9166=CARTESIAN_POINT('Ctrl Pts',(-0.22175178875163,2.99540054743711,0.894109450833571));
#9167=CARTESIAN_POINT('Ctrl Pts',(-0.592939587196475,3.0589070566873,0.717178592312595));
#9168=CARTESIAN_POINT('Ctrl Pts',(-0.853291005408645,3.12303606754463,0.393731991340956));
#9169=CARTESIAN_POINT('Ctrl Pts',(-0.948684337638334,3.18777770111288,-0.0144566266599512));
#9170=CARTESIAN_POINT('Ctrl Pts',(-0.856917921474516,3.25311897476409,-0.427457214656335));
#9171=CARTESIAN_POINT('Ctrl Pts',(-0.592906791304635,3.31904398316708,-0.762872291775904));
#9172=CARTESIAN_POINT('Ctrl Pts',(-0.206327696795635,3.38553401578509,-0.952349876980599));
#9173=CARTESIAN_POINT('Ctrl Pts',(0.227690644097483,3.45256754119835,-0.955627088535012));
#9174=CARTESIAN_POINT('Ctrl Pts',(0.623316753010274,3.52012024062849,-0.769024389527845));
#9175=CARTESIAN_POINT('Ctrl Pts',(0.900967743613051,3.58816512289236,-0.427008079610695));
#9176=CARTESIAN_POINT('Ctrl Pts',(1.00375079789027,3.65667314648915,0.00463978121626096));
#9177=CARTESIAN_POINT('Ctrl Pts',(0.908532101935272,3.72561178223024,0.440525826284625));
#9178=CARTESIAN_POINT('Ctrl Pts',(0.601976701053612,3.8026511284078,0.834343685753614));
#9179=CARTESIAN_POINT('Ctrl Pts',(0.0806362141225256,3.88792074321953,1.04632070591145));
#9180=CARTESIAN_POINT('Ctrl Pts',(-0.523620625967669,3.9815022105468,0.915840845262919));
#9181=CARTESIAN_POINT('Ctrl Pts',(-0.915935792656353,4.06771715054109,0.503867434474184));
#9182=CARTESIAN_POINT('Ctrl Pts',(-1.03518812510371,4.14634770587156,0.00846388977103227));
#9183=CARTESIAN_POINT('Ctrl Pts',(-0.939354725954324,4.21726768242631,-0.44039985190263));
#9184=CARTESIAN_POINT('Ctrl Pts',(-0.657622764287281,4.2883154938952,-0.804254512732454));
#9185=CARTESIAN_POINT('Ctrl Pts',(-0.29146462647341,4.35152846153295,-0.987256117242355));
#9186=CARTESIAN_POINT('Ctrl Pts',(0.0604069213856414,4.40687215270274,-1.01864808961705));
#9187=CARTESIAN_POINT('Ctrl Pts',(0.455817860274253,4.47011933657517,-0.935785288792637));
#9188=CARTESIAN_POINT('Ctrl Pts',(0.868997154316896,4.54914650202704,-0.617456627835253));
#9189=CARTESIAN_POINT('Ctrl Pts',(1.06333617461654,4.64382389525895,-0.0230756819531807));
#9190=CARTESIAN_POINT('Ctrl Pts',(0.890037371970145,4.73823988777768,0.575750516999619));
#9191=CARTESIAN_POINT('Ctrl Pts',(0.411621565129445,4.83230120305772,0.971758552342444));
#9192=CARTESIAN_POINT('Ctrl Pts',(-0.203757910870774,4.92589103507915,1.02970525192993));
#9193=CARTESIAN_POINT('Ctrl Pts',(-0.741665205819518,5.01895623726245,0.732797837240576));
#9194=CARTESIAN_POINT('Ctrl Pts',(-1.01747315988325,5.11132924690258,0.188632511506228));
#9195=CARTESIAN_POINT('Ctrl Pts',(-0.9398967031339,5.20307972080444,-0.411824505334644));
#9196=CARTESIAN_POINT('Ctrl Pts',(-0.541277959388034,5.29378223257878,-0.860029726746955));
#9197=CARTESIAN_POINT('Ctrl Pts',(0.0347131003179486,5.38416147101441,-1.00603962268195));
#9198=CARTESIAN_POINT('Ctrl Pts',(0.472449504710221,5.45393481550324,-0.844256072565711));
#9199=CARTESIAN_POINT('Ctrl Pts',(0.708109788427302,5.50633708994253,-0.620438326433588));
#9200=CARTESIAN_POINT('Ctrl Pts',(0.826310839284909,5.53916278990257,-0.441645104060546));
#9201=CARTESIAN_POINT('Ctrl Pts',(0.897616227875116,5.56964940189299,-0.253563543686594));
#9202=CARTESIAN_POINT('Ctrl Pts',(0.92297240476864,5.60448955322945,-0.0778455347175106));
#9203=CARTESIAN_POINT('Ctrl Pts',(0.918576908769613,5.61703094943253,0.073595424072634));
#9204=CARTESIAN_POINT('Ctrl Pts',(0.897813272525461,5.62033291313822,0.214442376647703));
#9205=CARTESIAN_POINT('Ctrl Pts',(0.84717914281391,5.62687408453863,0.372908518609524));
#9206=CARTESIAN_POINT('Ctrl Pts',(0.73902806886783,5.63938763900218,0.554930118177138));
#9207=CARTESIAN_POINT('Ctrl Pts',(0.54868329335707,5.65055047950713,0.754249110630997));
#9208=CARTESIAN_POINT('Ctrl Pts',(0.234740786310109,5.66833417008755,0.914319853294209));
#9209=CARTESIAN_POINT('Ctrl Pts',(-0.186280544388743,5.68698815338276,0.922248294213509));
#9210=CARTESIAN_POINT('Ctrl Pts',(-0.567738849793441,5.70701244501641,0.746989429520979));
#9211=CARTESIAN_POINT('Ctrl Pts',(-0.833876650451468,5.72630747686717,0.423805888181072));
#9212=CARTESIAN_POINT('Ctrl Pts',(-0.932393657693937,5.74583524156656,0.018270062398184));
#9213=CARTESIAN_POINT('Ctrl Pts',(-0.844669348182326,5.76516713174664,-0.388445981353963));
#9214=CARTESIAN_POINT('Ctrl Pts',(-0.589331567089245,5.78449854502205,-0.71541788303751));
#9215=CARTESIAN_POINT('Ctrl Pts',(-0.218194045974345,5.80374206815275,-0.897714376194275));
#9216=CARTESIAN_POINT('Ctrl Pts',(0.194035074001386,5.82293729736513,-0.900444896267203));
#9217=CARTESIAN_POINT('Ctrl Pts',(0.565131377847116,5.84206506652244,-0.723768454824322));
#9218=CARTESIAN_POINT('Ctrl Pts',(0.778569851413565,5.85796115725643,-0.457245638130952));
#9219=CARTESIAN_POINT('Ctrl Pts',(0.86699247800335,5.87063993939285,-0.20490166143947));
#9220=CARTESIAN_POINT('Ctrl Pts',(0.881970292931539,5.87697404420344,-0.0732444812903123));
#9221=CARTESIAN_POINT('Ctrl Pts',(0.882042267836621,5.88013978881747,-0.00614778728168446));
#9222=CARTESIAN_POINT('Ctrl Pts',(0.872161950711206,0.124828769264236,-0.00589269379913899));
#9223=CARTESIAN_POINT('Ctrl Pts',(0.872090904698941,0.127953657301625,0.0603380612992187));
#9224=CARTESIAN_POINT('Ctrl Pts',(0.857308714561314,0.134203213047992,0.190241275757611));
#9225=CARTESIAN_POINT('Ctrl Pts',(0.770187083636269,0.146690001256174,0.438769378299054));
#9226=CARTESIAN_POINT('Ctrl Pts',(0.560950745207346,0.162256028321672,0.699616259986153));
#9227=CARTESIAN_POINT('Ctrl Pts',(0.199511576340965,0.180880209711553,0.871422024437173));
#9228=CARTESIAN_POINT('Ctrl Pts',(-0.199312333389545,0.199448331926636,
0.868457819907934));
#9229=CARTESIAN_POINT('Ctrl Pts',(-0.556088930421348,0.217951986567579,
0.692928582783942));
#9230=CARTESIAN_POINT('Ctrl Pts',(-0.799862508003898,0.236416030436661,
0.380262416576452));
#9231=CARTESIAN_POINT('Ctrl Pts',(-0.882895646021795,0.254773193569333,
-0.0060546706614528));
#9232=CARTESIAN_POINT('Ctrl Pts',(-0.789649057445972,0.273182184223599,
-0.388883291654368));
#9233=CARTESIAN_POINT('Ctrl Pts',(-0.539659944242912,0.291280837799174,
-0.691764713311758));
#9234=CARTESIAN_POINT('Ctrl Pts',(-0.183956800223335,0.309860445327341,
-0.855316888413074));
#9235=CARTESIAN_POINT('Ctrl Pts',(0.206499015809491,0.327389549600143,-0.847162298078497));
#9236=CARTESIAN_POINT('Ctrl Pts',(0.49509577120488,0.34362645645855,-0.700495805282282));
#9237=CARTESIAN_POINT('Ctrl Pts',(0.670997034604971,0.353943958171212,-0.515417881277946));
#9238=CARTESIAN_POINT('Ctrl Pts',(0.766581438347442,0.365141873832304,-0.355537227212008));
#9239=CARTESIAN_POINT('Ctrl Pts',(0.8174676017473,0.371459915026287,-0.198233634126398));
#9240=CARTESIAN_POINT('Ctrl Pts',(0.834170515466371,0.374539492519685,-0.0771620442826736));
#9241=CARTESIAN_POINT('Ctrl Pts',(0.837719002104484,0.383704512647053,0.0354460071939376));
#9242=CARTESIAN_POINT('Ctrl Pts',(0.817405541799073,0.413175723298386,0.185924750839524));
#9243=CARTESIAN_POINT('Ctrl Pts',(0.748423543506377,0.44312071842525,0.367957985006333));
#9244=CARTESIAN_POINT('Ctrl Pts',(0.647340094288683,0.470691270109384,0.518903872562794));
#9245=CARTESIAN_POINT('Ctrl Pts',(0.466898254116811,0.511144063135416,0.691309623343175));
#9246=CARTESIAN_POINT('Ctrl Pts',(0.182800989155019,0.558222951408999,0.818397523700333));
#9247=CARTESIAN_POINT('Ctrl Pts',(-0.189545178060892,0.616501258086875,
0.809773850041606));
#9248=CARTESIAN_POINT('Ctrl Pts',(-0.462507583347405,0.663503908067788,
0.669357773844709));
#9249=CARTESIAN_POINT('Ctrl Pts',(-0.627863189228003,0.701318402481341,
0.495969553901588));
#9250=CARTESIAN_POINT('Ctrl Pts',(-0.750267427503473,0.738837453517587,
0.291088758101646));
#9251=CARTESIAN_POINT('Ctrl Pts',(-0.810712868559922,0.785528896923523,
-0.00492588128797676));
#9252=CARTESIAN_POINT('Ctrl Pts',(-0.722807305049749,0.841109138477463,
-0.35397737605765));
#9253=CARTESIAN_POINT('Ctrl Pts',(-0.493845277109899,0.896322143289524,
-0.6284699970223));
#9254=CARTESIAN_POINT('Ctrl Pts',(-0.170668331595556,0.951180240767939,
-0.77578162036287));
#9255=CARTESIAN_POINT('Ctrl Pts',(0.182411368712431,1.00572789901627,-0.768554583075931));
#9256=CARTESIAN_POINT('Ctrl Pts',(0.495894675031221,1.0599979812032,-0.609891173973463));
#9257=CARTESIAN_POINT('Ctrl Pts',(0.708755333326572,1.11403086100534,-0.332295680974433));
#9258=CARTESIAN_POINT('Ctrl Pts',(0.780070637830783,1.16786510347237,0.00885468431853584));
#9259=CARTESIAN_POINT('Ctrl Pts',(0.696791510479646,1.22154183082612,0.346232027663686));
#9260=CARTESIAN_POINT('Ctrl Pts',(0.476047266626745,1.27510240963086,0.61364355273423));
#9261=CARTESIAN_POINT('Ctrl Pts',(0.161678386661078,1.32858888114584,0.758820094473604));
#9262=CARTESIAN_POINT('Ctrl Pts',(-0.184345221885054,1.38204344182885,0.753472314023915));
#9263=CARTESIAN_POINT('Ctrl Pts',(-0.493955884546455,1.43550888318168,0.598711183433611));
#9264=CARTESIAN_POINT('Ctrl Pts',(-0.706164418456796,1.48902767046263,0.324820470310737));
#9265=CARTESIAN_POINT('Ctrl Pts',(-0.778894190579621,1.54264192169839,-0.0145743797186695));
#9266=CARTESIAN_POINT('Ctrl Pts',(-0.697192877485004,1.59639341722752,-0.352835018065878));
#9267=CARTESIAN_POINT('Ctrl Pts',(-0.476282548914222,1.65032345266182,-0.623209180930827));
#9268=CARTESIAN_POINT('Ctrl Pts',(-0.158743612035258,1.70447207761938,-0.771770092812482));
#9269=CARTESIAN_POINT('Ctrl Pts',(0.193450677004803,1.75887837965647,-0.768113401787862));
#9270=CARTESIAN_POINT('Ctrl Pts',(0.47579440943534,1.80750241451549,-0.628734440560694));
#9271=CARTESIAN_POINT('Ctrl Pts',(0.659272267850805,1.85026369378763,-0.426676852570877));
#9272=CARTESIAN_POINT('Ctrl Pts',(0.793229432459306,1.89934423589563,-0.143355198493509));
#9273=CARTESIAN_POINT('Ctrl Pts',(0.790263784307131,1.96111512092083,0.264407243055348));
#9274=CARTESIAN_POINT('Ctrl Pts',(0.532639208585251,2.02974904747753,0.637020032041957));
#9275=CARTESIAN_POINT('Ctrl Pts',(0.163609475192015,2.09273970975414,0.811198964310618));
#9276=CARTESIAN_POINT('Ctrl Pts',(-0.206325324489528,2.14991769756873,0.809290051602918));
#9277=CARTESIAN_POINT('Ctrl Pts',(-0.54210311156644,2.20760646525503,0.645493293137588));
#9278=CARTESIAN_POINT('Ctrl Pts',(-0.775793177879044,2.26582771180786,0.349801965195082));
#9279=CARTESIAN_POINT('Ctrl Pts',(-0.859118193146955,2.32460053758821,-0.0214433086745682));
#9280=CARTESIAN_POINT('Ctrl Pts',(-0.772497333242961,2.38394137391289,-0.395836964477112));
#9281=CARTESIAN_POINT('Ctrl Pts',(-0.529877815574135,2.44386394296014,-0.698375208084907));
#9282=CARTESIAN_POINT('Ctrl Pts',(-0.137454124419672,2.51110274201743,-0.887126219786336));
#9283=CARTESIAN_POINT('Ctrl Pts',(0.355020405406913,2.58592160387692,-0.85044216028401));
#9284=CARTESIAN_POINT('Ctrl Pts',(0.782180417385646,2.66862024366749,-0.50996194705241));
#9285=CARTESIAN_POINT('Ctrl Pts',(0.932029131507338,2.74541647960869,-0.0258957186176781));
#9286=CARTESIAN_POINT('Ctrl Pts',(0.830321215974015,2.81601192011723,0.419957402046343));
#9287=CARTESIAN_POINT('Ctrl Pts',(0.572400166827825,2.88014282443316,0.744989944459363));
#9288=CARTESIAN_POINT('Ctrl Pts',(0.195275509838113,2.94485897026784,0.927771382562365));
#9289=CARTESIAN_POINT('Ctrl Pts',(-0.227340767365424,3.01014754818103,0.929095017890615));
#9290=CARTESIAN_POINT('Ctrl Pts',(-0.612127646814787,3.07599293903656,0.745588291188903));
#9291=CARTESIAN_POINT('Ctrl Pts',(-0.881535208369304,3.14237676662695,0.410744646425331));
#9292=CARTESIAN_POINT('Ctrl Pts',(-0.980005185206354,3.20927820175596,-0.0110388926131081));
#9293=CARTESIAN_POINT('Ctrl Pts',(-0.885263395772081,3.27667359822412,-0.436952466191731));
#9294=CARTESIAN_POINT('Ctrl Pts',(-0.613436538369041,3.34453700325931,-0.782121048029494));
#9295=CARTESIAN_POINT('Ctrl Pts',(-0.216315847404239,3.41284022102408,-0.976638893510757));
#9296=CARTESIAN_POINT('Ctrl Pts',(0.228515688692952,3.48155290325642,-0.979879367890244));
#9297=CARTESIAN_POINT('Ctrl Pts',(0.633032334246116,3.55064249055004,-0.788946617304531));
#9298=CARTESIAN_POINT('Ctrl Pts',(0.91620307923501,3.62007471455624,-0.439929095068272));
#9299=CARTESIAN_POINT('Ctrl Pts',(1.02068551154318,3.6898138200776,-0.00055988972616793));
#9300=CARTESIAN_POINT('Ctrl Pts',(0.923874643413053,3.75982214337787,0.441983752855437));
#9301=CARTESIAN_POINT('Ctrl Pts',(0.613247660943624,3.83786518922612,0.840785019888275));
#9302=CARTESIAN_POINT('Ctrl Pts',(0.0866578234258063,3.9239844102579,1.05456997463629));
#9303=CARTESIAN_POINT('Ctrl Pts',(-0.521392660403112,4.01817435387289,0.92294994186792));
#9304=CARTESIAN_POINT('Ctrl Pts',(-0.914636612404499,4.10464567111125,0.509573712510557));
#9305=CARTESIAN_POINT('Ctrl Pts',(-1.03374180999006,4.18328650371776,0.0141535738014065));
#9306=CARTESIAN_POINT('Ctrl Pts',(-0.938026942329867,4.25404428614242,-0.433573776623787));
#9307=CARTESIAN_POINT('Ctrl Pts',(-0.657630260146868,4.32474041714926,-0.795496981882739));
#9308=CARTESIAN_POINT('Ctrl Pts',(-0.294187702113077,4.38748944604847,-0.977023505420508));
#9309=CARTESIAN_POINT('Ctrl Pts',(0.0542596632323615,4.44230054898675,-1.00807090756588));
#9310=CARTESIAN_POINT('Ctrl Pts',(0.445198581282316,4.50483969839108,-0.926094625208896));
#9311=CARTESIAN_POINT('Ctrl Pts',(0.852563310440807,4.58279123657346,-0.611941112564204));
#9312=CARTESIAN_POINT('Ctrl Pts',(1.04336115553597,4.67588518836249,-0.0274765552718303));
#9313=CARTESIAN_POINT('Ctrl Pts',(0.873243552350396,4.76843871793217,0.559396655291762));
#9314=CARTESIAN_POINT('Ctrl Pts',(0.405532574611691,4.86037265153526,0.946224142384314));
#9315=CARTESIAN_POINT('Ctrl Pts',(-0.194232561825003,4.95159408982323,1.00246182575268));
#9316=CARTESIAN_POINT('Ctrl Pts',(-0.716978005254575,5.04205915598986,0.713684974901636));
#9317=CARTESIAN_POINT('Ctrl Pts',(-0.984237521133288,5.13163619116299,0.185945073380498));
#9318=CARTESIAN_POINT('Ctrl Pts',(-0.909022704364039,5.22040809154829,-0.394980663551699));
#9319=CARTESIAN_POINT('Ctrl Pts',(-0.524008362921299,5.30799616173538,-0.827628543573509));
#9320=CARTESIAN_POINT('Ctrl Pts',(0.0311612934979211,5.39510126764713,-0.968284503878036));
#9321=CARTESIAN_POINT('Ctrl Pts',(0.452486451456519,5.46227744588555,-0.812413771015693));
#9322=CARTESIAN_POINT('Ctrl Pts',(0.678996914481602,5.51263767773254,-0.597335976683866));
#9323=CARTESIAN_POINT('Ctrl Pts',(0.792756702852497,5.54424482065645,-0.425194580715441));
#9324=CARTESIAN_POINT('Ctrl Pts',(0.861097079444627,5.57344984716716,-0.244943323368279));
#9325=CARTESIAN_POINT('Ctrl Pts',(0.885548394683697,5.6069898998326,-0.0758116878038518));
#9326=CARTESIAN_POINT('Ctrl Pts',(0.881311178103886,5.61908885250671,0.0702661570768112));
#9327=CARTESIAN_POINT('Ctrl Pts',(0.861324400417122,5.62225654974902,0.205633030471336));
#9328=CARTESIAN_POINT('Ctrl Pts',(0.812891366893097,5.62852110126019,0.357273663598819));
#9329=CARTESIAN_POINT('Ctrl Pts',(0.709033945858278,5.64053429758327,0.532105911493553));
#9330=CARTESIAN_POINT('Ctrl Pts',(0.526480038594941,5.65124067536637,0.723242801555853));
#9331=CARTESIAN_POINT('Ctrl Pts',(0.225331281496905,5.66829963228703,0.876812377650357));
#9332=CARTESIAN_POINT('Ctrl Pts',(-0.178438754359568,5.6861889761217,0.884400172818289));
#9333=CARTESIAN_POINT('Ctrl Pts',(-0.544244744848784,5.70539124964099,0.716342713969011));
#9334=CARTESIAN_POINT('Ctrl Pts',(-0.799436178683323,5.72389218103035,0.406445379440496));
#9335=CARTESIAN_POINT('Ctrl Pts',(-0.893901515434013,5.74261482334007,0.0176118727011753));
#9336=CARTESIAN_POINT('Ctrl Pts',(-0.809793026073925,5.76114914213192,-0.372336066624544));
#9337=CARTESIAN_POINT('Ctrl Pts',(-0.565009292976944,5.77968086993593,-0.685823620580416));
#9338=CARTESIAN_POINT('Ctrl Pts',(-0.209171565907703,5.79813086800354,-0.860593511818846));
#9339=CARTESIAN_POINT('Ctrl Pts',(0.186034384156284,5.8165319894943,-0.863241242665013));
#9340=CARTESIAN_POINT('Ctrl Pts',(0.541844299347737,5.83487223159308,-0.693819904186464));
#9341=CARTESIAN_POINT('Ctrl Pts',(0.746471713940332,5.85010991085684,-0.43833815015316));
#9342=CARTESIAN_POINT('Ctrl Pts',(0.831270497111571,5.86227119228351,-0.19628398706425));
#9343=CARTESIAN_POINT('Ctrl Pts',(0.845616258369985,5.86833999900766,-0.0701367303899257));
#9344=CARTESIAN_POINT('Ctrl Pts',(0.845685384742026,5.87138045372904,-0.00569550566726366));
#9345=CARTESIAN_POINT('',(0.872161950711206,0.124828769264236,-0.00589269379913899));
#9346=CARTESIAN_POINT('Origin',(0.875,0.,0.));
#9347=CARTESIAN_POINT('',(0.845685384742025,5.87138045372904,-0.00569550566726366));
#9348=CARTESIAN_POINT('Ctrl Pts',(0.872161950711206,0.124828769264236,-0.00589269379913899));
#9349=CARTESIAN_POINT('Ctrl Pts',(0.872090904698941,0.127953657301625,0.0603380612992187));
#9350=CARTESIAN_POINT('Ctrl Pts',(0.857308714561314,0.134203213047992,0.190241275757611));
#9351=CARTESIAN_POINT('Ctrl Pts',(0.770187083636269,0.146690001256174,0.438769378299054));
#9352=CARTESIAN_POINT('Ctrl Pts',(0.560950745207346,0.162256028321672,0.699616259986153));
#9353=CARTESIAN_POINT('Ctrl Pts',(0.199511576340965,0.180880209711553,0.871422024437173));
#9354=CARTESIAN_POINT('Ctrl Pts',(-0.199312333389545,0.199448331926636,
0.868457819907934));
#9355=CARTESIAN_POINT('Ctrl Pts',(-0.556088930421348,0.217951986567579,
0.692928582783942));
#9356=CARTESIAN_POINT('Ctrl Pts',(-0.799862508003898,0.236416030436661,
0.380262416576452));
#9357=CARTESIAN_POINT('Ctrl Pts',(-0.882895646021795,0.254773193569333,
-0.0060546706614528));
#9358=CARTESIAN_POINT('Ctrl Pts',(-0.789649057445972,0.273182184223599,
-0.388883291654368));
#9359=CARTESIAN_POINT('Ctrl Pts',(-0.539659944242912,0.291280837799174,
-0.691764713311758));
#9360=CARTESIAN_POINT('Ctrl Pts',(-0.183956800223335,0.309860445327341,
-0.855316888413074));
#9361=CARTESIAN_POINT('Ctrl Pts',(0.206499015809491,0.327389549600143,-0.847162298078497));
#9362=CARTESIAN_POINT('Ctrl Pts',(0.49509577120488,0.34362645645855,-0.700495805282282));
#9363=CARTESIAN_POINT('Ctrl Pts',(0.670997034604971,0.353943958171212,-0.515417881277946));
#9364=CARTESIAN_POINT('Ctrl Pts',(0.766581438347442,0.365141873832304,-0.355537227212008));
#9365=CARTESIAN_POINT('Ctrl Pts',(0.8174676017473,0.371459915026287,-0.198233634126398));
#9366=CARTESIAN_POINT('Ctrl Pts',(0.834170515466371,0.374539492519685,-0.0771620442826736));
#9367=CARTESIAN_POINT('Ctrl Pts',(0.837719002104484,0.383704512647053,0.0354460071939376));
#9368=CARTESIAN_POINT('Ctrl Pts',(0.817405541799073,0.413175723298386,0.185924750839524));
#9369=CARTESIAN_POINT('Ctrl Pts',(0.748423543506377,0.44312071842525,0.367957985006333));
#9370=CARTESIAN_POINT('Ctrl Pts',(0.647340094288683,0.470691270109384,0.518903872562794));
#9371=CARTESIAN_POINT('Ctrl Pts',(0.466898254116811,0.511144063135416,0.691309623343175));
#9372=CARTESIAN_POINT('Ctrl Pts',(0.182800989155019,0.558222951408999,0.818397523700333));
#9373=CARTESIAN_POINT('Ctrl Pts',(-0.189545178060892,0.616501258086875,
0.809773850041606));
#9374=CARTESIAN_POINT('Ctrl Pts',(-0.462507583347405,0.663503908067788,
0.669357773844709));
#9375=CARTESIAN_POINT('Ctrl Pts',(-0.627863189228003,0.701318402481341,
0.495969553901588));
#9376=CARTESIAN_POINT('Ctrl Pts',(-0.750267427503473,0.738837453517587,
0.291088758101646));
#9377=CARTESIAN_POINT('Ctrl Pts',(-0.810712868559922,0.785528896923523,
-0.00492588128797676));
#9378=CARTESIAN_POINT('Ctrl Pts',(-0.722807305049749,0.841109138477463,
-0.35397737605765));
#9379=CARTESIAN_POINT('Ctrl Pts',(-0.493845277109899,0.896322143289524,
-0.6284699970223));
#9380=CARTESIAN_POINT('Ctrl Pts',(-0.170668331595556,0.951180240767939,
-0.77578162036287));
#9381=CARTESIAN_POINT('Ctrl Pts',(0.182411368712431,1.00572789901627,-0.768554583075931));
#9382=CARTESIAN_POINT('Ctrl Pts',(0.495894675031221,1.0599979812032,-0.609891173973463));
#9383=CARTESIAN_POINT('Ctrl Pts',(0.708755333326572,1.11403086100534,-0.332295680974433));
#9384=CARTESIAN_POINT('Ctrl Pts',(0.780070637830783,1.16786510347237,0.00885468431853584));
#9385=CARTESIAN_POINT('Ctrl Pts',(0.696791510479646,1.22154183082612,0.346232027663686));
#9386=CARTESIAN_POINT('Ctrl Pts',(0.476047266626745,1.27510240963086,0.61364355273423));
#9387=CARTESIAN_POINT('Ctrl Pts',(0.161678386661078,1.32858888114584,0.758820094473604));
#9388=CARTESIAN_POINT('Ctrl Pts',(-0.184345221885054,1.38204344182885,0.753472314023915));
#9389=CARTESIAN_POINT('Ctrl Pts',(-0.493955884546455,1.43550888318168,0.598711183433611));
#9390=CARTESIAN_POINT('Ctrl Pts',(-0.706164418456796,1.48902767046263,0.324820470310737));
#9391=CARTESIAN_POINT('Ctrl Pts',(-0.778894190579621,1.54264192169839,-0.0145743797186695));
#9392=CARTESIAN_POINT('Ctrl Pts',(-0.697192877485004,1.59639341722752,-0.352835018065878));
#9393=CARTESIAN_POINT('Ctrl Pts',(-0.476282548914222,1.65032345266182,-0.623209180930827));
#9394=CARTESIAN_POINT('Ctrl Pts',(-0.158743612035258,1.70447207761938,-0.771770092812482));
#9395=CARTESIAN_POINT('Ctrl Pts',(0.193450677004803,1.75887837965647,-0.768113401787862));
#9396=CARTESIAN_POINT('Ctrl Pts',(0.47579440943534,1.80750241451549,-0.628734440560694));
#9397=CARTESIAN_POINT('Ctrl Pts',(0.659272267850805,1.85026369378763,-0.426676852570877));
#9398=CARTESIAN_POINT('Ctrl Pts',(0.793229432459306,1.89934423589563,-0.143355198493509));
#9399=CARTESIAN_POINT('Ctrl Pts',(0.790263784307131,1.96111512092083,0.264407243055348));
#9400=CARTESIAN_POINT('Ctrl Pts',(0.532639208585251,2.02974904747753,0.637020032041957));
#9401=CARTESIAN_POINT('Ctrl Pts',(0.163609475192015,2.09273970975414,0.811198964310618));
#9402=CARTESIAN_POINT('Ctrl Pts',(-0.206325324489528,2.14991769756873,0.809290051602918));
#9403=CARTESIAN_POINT('Ctrl Pts',(-0.54210311156644,2.20760646525503,0.645493293137588));
#9404=CARTESIAN_POINT('Ctrl Pts',(-0.775793177879044,2.26582771180786,0.349801965195082));
#9405=CARTESIAN_POINT('Ctrl Pts',(-0.859118193146955,2.32460053758821,-0.0214433086745682));
#9406=CARTESIAN_POINT('Ctrl Pts',(-0.772497333242961,2.38394137391289,-0.395836964477112));
#9407=CARTESIAN_POINT('Ctrl Pts',(-0.529877815574135,2.44386394296014,-0.698375208084907));
#9408=CARTESIAN_POINT('Ctrl Pts',(-0.137454124419672,2.51110274201743,-0.887126219786336));
#9409=CARTESIAN_POINT('Ctrl Pts',(0.355020405406913,2.58592160387692,-0.85044216028401));
#9410=CARTESIAN_POINT('Ctrl Pts',(0.782180417385646,2.66862024366749,-0.50996194705241));
#9411=CARTESIAN_POINT('Ctrl Pts',(0.932029131507338,2.74541647960869,-0.0258957186176781));
#9412=CARTESIAN_POINT('Ctrl Pts',(0.830321215974015,2.81601192011723,0.419957402046343));
#9413=CARTESIAN_POINT('Ctrl Pts',(0.572400166827825,2.88014282443316,0.744989944459363));
#9414=CARTESIAN_POINT('Ctrl Pts',(0.195275509838113,2.94485897026784,0.927771382562365));
#9415=CARTESIAN_POINT('Ctrl Pts',(-0.227340767365424,3.01014754818103,0.929095017890615));
#9416=CARTESIAN_POINT('Ctrl Pts',(-0.612127646814787,3.07599293903656,0.745588291188903));
#9417=CARTESIAN_POINT('Ctrl Pts',(-0.881535208369304,3.14237676662695,0.410744646425331));
#9418=CARTESIAN_POINT('Ctrl Pts',(-0.980005185206354,3.20927820175596,-0.0110388926131081));
#9419=CARTESIAN_POINT('Ctrl Pts',(-0.885263395772081,3.27667359822412,-0.436952466191731));
#9420=CARTESIAN_POINT('Ctrl Pts',(-0.613436538369041,3.34453700325931,-0.782121048029494));
#9421=CARTESIAN_POINT('Ctrl Pts',(-0.216315847404239,3.41284022102408,-0.976638893510757));
#9422=CARTESIAN_POINT('Ctrl Pts',(0.228515688692952,3.48155290325642,-0.979879367890244));
#9423=CARTESIAN_POINT('Ctrl Pts',(0.633032334246116,3.55064249055004,-0.788946617304531));
#9424=CARTESIAN_POINT('Ctrl Pts',(0.91620307923501,3.62007471455624,-0.439929095068272));
#9425=CARTESIAN_POINT('Ctrl Pts',(1.02068551154318,3.6898138200776,-0.00055988972616793));
#9426=CARTESIAN_POINT('Ctrl Pts',(0.923874643413053,3.75982214337787,0.441983752855437));
#9427=CARTESIAN_POINT('Ctrl Pts',(0.613247660943624,3.83786518922612,0.840785019888275));
#9428=CARTESIAN_POINT('Ctrl Pts',(0.0866578234258063,3.9239844102579,1.05456997463629));
#9429=CARTESIAN_POINT('Ctrl Pts',(-0.521392660403112,4.01817435387289,0.92294994186792));
#9430=CARTESIAN_POINT('Ctrl Pts',(-0.914636612404499,4.10464567111125,0.509573712510557));
#9431=CARTESIAN_POINT('Ctrl Pts',(-1.03374180999006,4.18328650371776,0.0141535738014065));
#9432=CARTESIAN_POINT('Ctrl Pts',(-0.938026942329867,4.25404428614242,-0.433573776623787));
#9433=CARTESIAN_POINT('Ctrl Pts',(-0.657630260146868,4.32474041714926,-0.795496981882739));
#9434=CARTESIAN_POINT('Ctrl Pts',(-0.294187702113077,4.38748944604847,-0.977023505420508));
#9435=CARTESIAN_POINT('Ctrl Pts',(0.0542596632323615,4.44230054898675,-1.00807090756588));
#9436=CARTESIAN_POINT('Ctrl Pts',(0.445198581282316,4.50483969839108,-0.926094625208896));
#9437=CARTESIAN_POINT('Ctrl Pts',(0.852563310440807,4.58279123657346,-0.611941112564204));
#9438=CARTESIAN_POINT('Ctrl Pts',(1.04336115553597,4.67588518836249,-0.0274765552718303));
#9439=CARTESIAN_POINT('Ctrl Pts',(0.873243552350396,4.76843871793217,0.559396655291762));
#9440=CARTESIAN_POINT('Ctrl Pts',(0.405532574611691,4.86037265153526,0.946224142384314));
#9441=CARTESIAN_POINT('Ctrl Pts',(-0.194232561825003,4.95159408982323,1.00246182575268));
#9442=CARTESIAN_POINT('Ctrl Pts',(-0.716978005254575,5.04205915598986,0.713684974901636));
#9443=CARTESIAN_POINT('Ctrl Pts',(-0.984237521133288,5.13163619116299,0.185945073380498));
#9444=CARTESIAN_POINT('Ctrl Pts',(-0.909022704364039,5.22040809154829,-0.394980663551699));
#9445=CARTESIAN_POINT('Ctrl Pts',(-0.524008362921299,5.30799616173538,-0.827628543573509));
#9446=CARTESIAN_POINT('Ctrl Pts',(0.0311612934979211,5.39510126764713,-0.968284503878036));
#9447=CARTESIAN_POINT('Ctrl Pts',(0.452486451456519,5.46227744588555,-0.812413771015693));
#9448=CARTESIAN_POINT('Ctrl Pts',(0.678996914481602,5.51263767773254,-0.597335976683866));
#9449=CARTESIAN_POINT('Ctrl Pts',(0.792756702852497,5.54424482065645,-0.425194580715441));
#9450=CARTESIAN_POINT('Ctrl Pts',(0.861097079444627,5.57344984716716,-0.244943323368279));
#9451=CARTESIAN_POINT('Ctrl Pts',(0.885548394683697,5.6069898998326,-0.0758116878038518));
#9452=CARTESIAN_POINT('Ctrl Pts',(0.881311178103886,5.61908885250671,0.0702661570768112));
#9453=CARTESIAN_POINT('Ctrl Pts',(0.861324400417122,5.62225654974902,0.205633030471336));
#9454=CARTESIAN_POINT('Ctrl Pts',(0.812891366893097,5.62852110126019,0.357273663598819));
#9455=CARTESIAN_POINT('Ctrl Pts',(0.709033945858278,5.64053429758327,0.532105911493553));
#9456=CARTESIAN_POINT('Ctrl Pts',(0.526480038594941,5.65124067536637,0.723242801555853));
#9457=CARTESIAN_POINT('Ctrl Pts',(0.225331281496905,5.66829963228703,0.876812377650357));
#9458=CARTESIAN_POINT('Ctrl Pts',(-0.178438754359568,5.6861889761217,0.884400172818289));
#9459=CARTESIAN_POINT('Ctrl Pts',(-0.544244744848784,5.70539124964099,0.716342713969011));
#9460=CARTESIAN_POINT('Ctrl Pts',(-0.799436178683323,5.72389218103035,0.406445379440496));
#9461=CARTESIAN_POINT('Ctrl Pts',(-0.893901515434013,5.74261482334007,0.0176118727011753));
#9462=CARTESIAN_POINT('Ctrl Pts',(-0.809793026073925,5.76114914213192,-0.372336066624544));
#9463=CARTESIAN_POINT('Ctrl Pts',(-0.565009292976944,5.77968086993593,-0.685823620580416));
#9464=CARTESIAN_POINT('Ctrl Pts',(-0.209171565907703,5.79813086800354,-0.860593511818846));
#9465=CARTESIAN_POINT('Ctrl Pts',(0.186034384156284,5.8165319894943,-0.863241242665013));
#9466=CARTESIAN_POINT('Ctrl Pts',(0.541844299347737,5.83487223159308,-0.693819904186464));
#9467=CARTESIAN_POINT('Ctrl Pts',(0.746471713940332,5.85010991085684,-0.43833815015316));
#9468=CARTESIAN_POINT('Ctrl Pts',(0.831270497111571,5.86227119228351,-0.19628398706425));
#9469=CARTESIAN_POINT('Ctrl Pts',(0.845616258369985,5.86833999900766,-0.0701367303899257));
#9470=CARTESIAN_POINT('Ctrl Pts',(0.845685384742026,5.87138045372904,-0.00569550566726366));
#9471=CARTESIAN_POINT('Origin',(0.875,5.74999999999999,1.53717316653257E-13));
#9472=CARTESIAN_POINT('Origin',(0.875,5.74999999999999,1.53717316653257E-13));
#9473=CARTESIAN_POINT('Origin',(0.875,0.,0.));
#9474=CARTESIAN_POINT('',(0.,0.,0.));
#9475=CARTESIAN_POINT('Origin',(0.,5.3,10.59));
#9476=CARTESIAN_POINT('',(0.133884278389952,5.13821310312636,10.59));
#9477=CARTESIAN_POINT('',(0.133884278389952,5.46178689687364,10.59));
#9478=CARTESIAN_POINT('',(0.133884278389952,4.9,10.59));
#9479=CARTESIAN_POINT('Origin',(0.,5.3,10.59));
#9480=CARTESIAN_POINT('Origin',(0.,5.3,10.59));
#9481=CARTESIAN_POINT('',(-0.133884278389952,5.13821310312636,10.59));
#9482=CARTESIAN_POINT('Ctrl Pts',(-0.133884278389952,5.13821310312636,10.59));
#9483=CARTESIAN_POINT('Ctrl Pts',(-0.118254395260799,5.12527883178237,10.5935467722442));
#9484=CARTESIAN_POINT('Ctrl Pts',(-0.100109787682297,5.11420068341256,10.5969822478996));
#9485=CARTESIAN_POINT('Ctrl Pts',(-0.0548298721325188,5.09536143894557,
10.6030741628997));
#9486=CARTESIAN_POINT('Ctrl Pts',(-0.0266020595922903,5.09,10.605));
#9487=CARTESIAN_POINT('Ctrl Pts',(0.0266020595922903,5.09,10.605));
#9488=CARTESIAN_POINT('Ctrl Pts',(0.0548298721325188,5.09536143894557,10.6030741628997));
#9489=CARTESIAN_POINT('Ctrl Pts',(0.100109787682297,5.11420068341256,10.5969822478996));
#9490=CARTESIAN_POINT('Ctrl Pts',(0.118254395260799,5.12527883178237,10.5935467722442));
#9491=CARTESIAN_POINT('Ctrl Pts',(0.133884278389952,5.13821310312636,10.59));
#9492=CARTESIAN_POINT('',(-0.21,5.3,10.59));
#9493=CARTESIAN_POINT('Origin',(0.,5.3,10.59));
#9494=CARTESIAN_POINT('',(-0.21,5.3,11.0797684937059));
#9495=CARTESIAN_POINT('',(-0.21,5.3,10.59));
#9496=CARTESIAN_POINT('',(0.21,5.3,11.0797684937059));
#9497=CARTESIAN_POINT('Ctrl Pts',(0.21,5.3,11.0797684937059));
#9498=CARTESIAN_POINT('Ctrl Pts',(0.21,5.27356141186949,11.0797684937059));
#9499=CARTESIAN_POINT('Ctrl Pts',(0.204702922670976,5.24540621874507,11.0808401566467));
#9500=CARTESIAN_POINT('Ctrl Pts',(0.183251796806354,5.19368655445866,11.0846831370713));
#9501=CARTESIAN_POINT('Ctrl Pts',(0.167101177357215,5.17011632925886,11.0873959305462));
#9502=CARTESIAN_POINT('Ctrl Pts',(0.129884533480965,5.13289968538261,11.0924663328912));
#9503=CARTESIAN_POINT('Ctrl Pts',(0.106313940757289,5.11674838983659,11.0951573889536));
#9504=CARTESIAN_POINT('Ctrl Pts',(0.0545930033295207,5.09529677343026,11.0989503922059));
#9505=CARTESIAN_POINT('Ctrl Pts',(0.0264373623835353,5.09,11.1));
#9506=CARTESIAN_POINT('Ctrl Pts',(-0.0264373623835352,5.09,11.1));
#9507=CARTESIAN_POINT('Ctrl Pts',(-0.0545930033295207,5.09529677343026,
11.0989503922059));
#9508=CARTESIAN_POINT('Ctrl Pts',(-0.106313940757289,5.11674838983659,11.0951573889536));
#9509=CARTESIAN_POINT('Ctrl Pts',(-0.129884533480965,5.13289968538261,11.0924663328912));
#9510=CARTESIAN_POINT('Ctrl Pts',(-0.167101177357215,5.17011632925886,11.0873959305462));
#9511=CARTESIAN_POINT('Ctrl Pts',(-0.183251796806354,5.19368655445866,11.0846831370713));
#9512=CARTESIAN_POINT('Ctrl Pts',(-0.204702922670976,5.24540621874507,11.0808401566467));
#9513=CARTESIAN_POINT('Ctrl Pts',(-0.21,5.27356141186949,11.0797684937059));
#9514=CARTESIAN_POINT('Ctrl Pts',(-0.21,5.3,11.0797684937059));
#9515=CARTESIAN_POINT('Ctrl Pts',(-0.21,5.3,11.0797684937059));
#9516=CARTESIAN_POINT('Ctrl Pts',(-0.21,5.32643858813051,11.0797684937059));
#9517=CARTESIAN_POINT('Ctrl Pts',(-0.204702922670976,5.35459378125493,11.0808401566467));
#9518=CARTESIAN_POINT('Ctrl Pts',(-0.183251796806354,5.40631344554134,11.0846831370713));
#9519=CARTESIAN_POINT('Ctrl Pts',(-0.167101177357215,5.42988367074114,11.0873959305462));
#9520=CARTESIAN_POINT('Ctrl Pts',(-0.129884533480965,5.46710031461738,11.0924663328912));
#9521=CARTESIAN_POINT('Ctrl Pts',(-0.106313940757289,5.48325161016341,11.0951573889536));
#9522=CARTESIAN_POINT('Ctrl Pts',(-0.0545930033295208,5.50470322656974,
11.0989503922059));
#9523=CARTESIAN_POINT('Ctrl Pts',(-0.0264373623835353,5.51,11.1));
#9524=CARTESIAN_POINT('Ctrl Pts',(0.0264373623835352,5.51,11.1));
#9525=CARTESIAN_POINT('Ctrl Pts',(0.0545930033295208,5.50470322656974,11.0989503922059));
#9526=CARTESIAN_POINT('Ctrl Pts',(0.106313940757289,5.48325161016341,11.0951573889536));
#9527=CARTESIAN_POINT('Ctrl Pts',(0.129884533480965,5.46710031461738,11.0924663328912));
#9528=CARTESIAN_POINT('Ctrl Pts',(0.167101177357214,5.42988367074114,11.0873959305462));
#9529=CARTESIAN_POINT('Ctrl Pts',(0.183251796806354,5.40631344554134,11.0846831370713));
#9530=CARTESIAN_POINT('Ctrl Pts',(0.204702922670976,5.35459378125493,11.0808401566467));
#9531=CARTESIAN_POINT('Ctrl Pts',(0.21,5.32643858813051,11.0797684937059));
#9532=CARTESIAN_POINT('Ctrl Pts',(0.21,5.3,11.0797684937059));
#9533=CARTESIAN_POINT('',(-0.133884278389952,5.46178689687364,10.59));
#9534=CARTESIAN_POINT('Origin',(0.,5.3,10.59));
#9535=CARTESIAN_POINT('Ctrl Pts',(0.133884278389952,5.46178689687364,10.59));
#9536=CARTESIAN_POINT('Ctrl Pts',(0.118254395260798,5.47472116821763,10.5935467722442));
#9537=CARTESIAN_POINT('Ctrl Pts',(0.100109787682297,5.48579931658744,10.5969822478996));
#9538=CARTESIAN_POINT('Ctrl Pts',(0.0548298721325188,5.50463856105443,10.6030741628997));
#9539=CARTESIAN_POINT('Ctrl Pts',(0.0266020595922903,5.51,10.605));
#9540=CARTESIAN_POINT('Ctrl Pts',(-0.0266020595922903,5.51,10.605));
#9541=CARTESIAN_POINT('Ctrl Pts',(-0.0548298721325188,5.50463856105443,
10.6030741628997));
#9542=CARTESIAN_POINT('Ctrl Pts',(-0.100109787682297,5.48579931658744,10.5969822478996));
#9543=CARTESIAN_POINT('Ctrl Pts',(-0.118254395260799,5.47472116821763,10.5935467722442));
#9544=CARTESIAN_POINT('Ctrl Pts',(-0.133884278389952,5.46178689687364,10.59));
#9545=CARTESIAN_POINT('Origin',(0.,5.3,10.59));
#9546=CARTESIAN_POINT('',(-0.133884278389952,4.9,10.59));
#9547=CARTESIAN_POINT('Origin',(0.,4.9,10.));
#9548=CARTESIAN_POINT('',(-0.605,5.7,10.));
#9549=CARTESIAN_POINT('Origin',(0.,5.7,10.));
#9550=CARTESIAN_POINT('',(-0.605,4.9,10.));
#9551=CARTESIAN_POINT('',(-0.605,4.9,10.));
#9552=CARTESIAN_POINT('Origin',(0.,4.9,10.));
#9553=CARTESIAN_POINT('Origin',(0.,4.9,10.));
#9554=CARTESIAN_POINT('',(-1.1,5.7,10.));
#9555=CARTESIAN_POINT('Origin',(0.,5.7,10.));
#9556=CARTESIAN_POINT('',(-1.1,4.9,10.));
#9557=CARTESIAN_POINT('',(-1.1,4.9,10.));
#9558=CARTESIAN_POINT('Origin',(0.,4.9,10.));
#9559=CARTESIAN_POINT('Origin',(0.,5.7,10.));
#9560=CARTESIAN_POINT('Origin',(0.,4.9,10.));
#9561=CARTESIAN_POINT('',(0.,0.,0.));
#9562=CARTESIAN_POINT('Origin',(0.0721687836487032,0.,-0.125));
#9563=CARTESIAN_POINT('',(0.0721687836487032,0.,-0.125));
#9564=CARTESIAN_POINT('',(0.144337567297406,0.,0.));
#9565=CARTESIAN_POINT('',(0.117710979560879,0.,-0.0461186027918559));
#9566=CARTESIAN_POINT('',(0.0721687836487032,-0.25,-0.125));
#9567=CARTESIAN_POINT('',(0.0721687836487032,0.,-0.125));
#9568=CARTESIAN_POINT('',(0.144337567297406,-0.25,0.));
#9569=CARTESIAN_POINT('',(0.144337567297406,-0.25,0.));
#9570=CARTESIAN_POINT('',(0.144337567297406,0.,0.));
#9571=CARTESIAN_POINT('Origin',(-0.0721687836487032,0.,-0.125));
#9572=CARTESIAN_POINT('',(-0.0721687836487032,0.,-0.125));
#9573=CARTESIAN_POINT('',(0.0739156081756484,0.,-0.125));
#9574=CARTESIAN_POINT('',(-0.0721687836487032,-0.25,-0.125));
#9575=CARTESIAN_POINT('',(-0.0721687836487032,0.,-0.125));
#9576=CARTESIAN_POINT('',(0.0721687836487032,-0.25,-0.125));
#9577=CARTESIAN_POINT('Origin',(-0.144337567297406,0.,-4.16333634234434E-17));
#9578=CARTESIAN_POINT('',(-0.144337567297406,0.,-1.76762539787485E-17));
#9579=CARTESIAN_POINT('',(-0.0987953713852306,0.,-0.0788813972081442));
#9580=CARTESIAN_POINT('',(-0.144337567297406,-0.25,-2.77555756156289E-17));
#9581=CARTESIAN_POINT('',(-0.144337567297406,0.,-1.76762539787485E-17));
#9582=CARTESIAN_POINT('',(-0.0721687836487032,-0.25,-0.125));
#9583=CARTESIAN_POINT('Origin',(-0.0721687836487033,0.,0.125));
#9584=CARTESIAN_POINT('',(-0.0721687836487033,0.,0.125));
#9585=CARTESIAN_POINT('',(-0.0627109795608791,0.,0.141381397208144));
#9586=CARTESIAN_POINT('',(-0.0721687836487033,-0.25,0.125));
#9587=CARTESIAN_POINT('',(-0.0721687836487033,0.,0.125));
#9588=CARTESIAN_POINT('',(-0.144337567297406,-0.25,-1.76762539787485E-17));
#9589=CARTESIAN_POINT('Origin',(0.0721687836487032,0.,0.125));
#9590=CARTESIAN_POINT('',(0.0721687836487032,0.,0.125));
#9591=CARTESIAN_POINT('',(0.146084391824352,0.,0.125));
#9592=CARTESIAN_POINT('',(0.0721687836487032,-0.25,0.125));
#9593=CARTESIAN_POINT('',(0.0721687836487032,0.,0.125));
#9594=CARTESIAN_POINT('',(-0.0721687836487033,-0.25,0.125));
#9595=CARTESIAN_POINT('Origin',(0.144337567297406,0.,0.));
#9596=CARTESIAN_POINT('',(0.153795371385231,0.,-0.0163813972081441));
#9597=CARTESIAN_POINT('',(0.0721687836487032,-0.25,0.125));
#9598=CARTESIAN_POINT('Origin',(0.,-0.25,0.));
#9599=CARTESIAN_POINT('Origin',(0.22,0.,0.));
#9600=CARTESIAN_POINT('',(-0.22,-8.67361737988404E-18,-2.69422295812418E-17));
#9601=CARTESIAN_POINT('Origin',(0.,0.,0.));
#9602=CARTESIAN_POINT('Origin',(0.,-0.015,0.));
#9603=CARTESIAN_POINT('',(-0.24505,-0.02505,-3.00099698131059E-17));
#9604=CARTESIAN_POINT('Origin',(0.,-0.02505,0.));
#9605=CARTESIAN_POINT('',(-0.235,-0.015,-2.87791997799628E-17));
#9606=CARTESIAN_POINT('Origin',(0.,-0.3775,0.));
#9607=CARTESIAN_POINT('',(-0.24505,-0.72995,3.00099698131059E-17));
#9608=CARTESIAN_POINT('Origin',(0.,-0.72995,0.));
#9609=CARTESIAN_POINT('',(-0.24505,-0.3775,-3.00099698131059E-17));
#9610=CARTESIAN_POINT('Origin',(0.,-0.7625,0.));
#9611=CARTESIAN_POINT('',(-0.175,-0.8,-2.14313189850787E-17));
#9612=CARTESIAN_POINT('Origin',(0.,-0.8,0.));
#9613=CARTESIAN_POINT('',(-0.2125,-0.7625,-2.60237444818813E-17));
#9614=CARTESIAN_POINT('Origin',(0.,-0.8,0.));
#9615=CARTESIAN_POINT('',(0.,0.,0.));
#9616=CARTESIAN_POINT('',(0.,0.,0.));
#9617=CARTESIAN_POINT('Origin',(13.4,5.5,3.));
#9618=CARTESIAN_POINT('',(13.5,5.5,3.165));
#9619=CARTESIAN_POINT('Origin',(13.5,5.5,3.));
#9620=CARTESIAN_POINT('',(16.5,5.5,3.165));
#9621=CARTESIAN_POINT('',(13.4,5.5,3.165));
#9622=CARTESIAN_POINT('Origin',(16.5,5.5,3.));
#9623=CARTESIAN_POINT('Origin',(13.4,-5.5,5.));
#9624=CARTESIAN_POINT('',(13.5,-5.5,5.165));
#9625=CARTESIAN_POINT('Origin',(13.5,-5.5,5.));
#9626=CARTESIAN_POINT('',(16.5,-5.5,5.165));
#9627=CARTESIAN_POINT('',(13.4,-5.5,5.165));
#9628=CARTESIAN_POINT('Origin',(16.5,-5.5,5.));
#9629=CARTESIAN_POINT('Origin',(13.4,-5.5,3.));
#9630=CARTESIAN_POINT('',(13.5,-5.5,3.165));
#9631=CARTESIAN_POINT('Origin',(13.5,-5.5,3.));
#9632=CARTESIAN_POINT('',(16.5,-5.5,3.165));
#9633=CARTESIAN_POINT('',(13.4,-5.5,3.165));
#9634=CARTESIAN_POINT('Origin',(16.5,-5.5,3.));
#9635=CARTESIAN_POINT('Origin',(13.4,5.5,5.));
#9636=CARTESIAN_POINT('',(13.5,5.5,5.165));
#9637=CARTESIAN_POINT('Origin',(13.5,5.5,5.));
#9638=CARTESIAN_POINT('',(16.5,5.5,5.165));
#9639=CARTESIAN_POINT('',(13.4,5.5,5.165));
#9640=CARTESIAN_POINT('Origin',(16.5,5.5,5.));
#9641=CARTESIAN_POINT('Origin',(16.,-2.2,4.4));
#9642=CARTESIAN_POINT('',(15.79,-2.2,4.4));
#9643=CARTESIAN_POINT('Origin',(16.,-2.2,4.4));
#9644=CARTESIAN_POINT('',(15.79,-2.2,5.8));
#9645=CARTESIAN_POINT('',(15.79,-2.2,4.4));
#9646=CARTESIAN_POINT('Origin',(16.,-2.2,5.8));
#9647=CARTESIAN_POINT('Origin',(16.,-2.2,4.4));
#9648=CARTESIAN_POINT('Origin',(14.,2.2,4.4));
#9649=CARTESIAN_POINT('',(13.79,2.2,4.4));
#9650=CARTESIAN_POINT('Origin',(14.,2.2,4.4));
#9651=CARTESIAN_POINT('',(13.79,2.2,5.8));
#9652=CARTESIAN_POINT('',(13.79,2.2,4.4));
#9653=CARTESIAN_POINT('Origin',(14.,2.2,5.8));
#9654=CARTESIAN_POINT('Origin',(14.,2.2,4.4));
#9655=CARTESIAN_POINT('Origin',(14.,-2.2,4.4));
#9656=CARTESIAN_POINT('',(13.79,-2.2,4.4));
#9657=CARTESIAN_POINT('Origin',(14.,-2.2,4.4));
#9658=CARTESIAN_POINT('',(13.79,-2.2,5.8));
#9659=CARTESIAN_POINT('',(13.79,-2.2,4.4));
#9660=CARTESIAN_POINT('Origin',(14.,-2.2,5.8));
#9661=CARTESIAN_POINT('Origin',(14.,-2.2,4.4));
#9662=CARTESIAN_POINT('Origin',(16.,2.2,4.4));
#9663=CARTESIAN_POINT('',(15.79,2.2,4.4));
#9664=CARTESIAN_POINT('Origin',(16.,2.2,4.4));
#9665=CARTESIAN_POINT('',(15.79,2.2,5.8));
#9666=CARTESIAN_POINT('',(15.79,2.2,4.4));
#9667=CARTESIAN_POINT('Origin',(16.,2.2,5.8));
#9668=CARTESIAN_POINT('Origin',(16.,2.2,4.4));
#9669=CARTESIAN_POINT('Origin',(13.4,-4.,3.3));
#9670=CARTESIAN_POINT('',(13.5,-4.,4.35));
#9671=CARTESIAN_POINT('Origin',(13.5,-4.,3.3));
#9672=CARTESIAN_POINT('',(16.5,-4.,4.35));
#9673=CARTESIAN_POINT('',(13.4,-4.,4.35));
#9674=CARTESIAN_POINT('Origin',(16.5,-4.,3.3));
#9675=CARTESIAN_POINT('Origin',(13.4,4.,3.3));
#9676=CARTESIAN_POINT('',(13.5,4.,4.35));
#9677=CARTESIAN_POINT('Origin',(13.5,4.,3.3));
#9678=CARTESIAN_POINT('',(16.5,4.,4.35));
#9679=CARTESIAN_POINT('',(13.4,4.,4.35));
#9680=CARTESIAN_POINT('Origin',(16.5,4.,3.3));
#9681=CARTESIAN_POINT('Origin',(16.5,6.,1.6));
#9682=CARTESIAN_POINT('',(16.5,6.,1.6));
#9683=CARTESIAN_POINT('',(13.5,6.,1.6));
#9684=CARTESIAN_POINT('',(16.5,6.,1.6));
#9685=CARTESIAN_POINT('',(13.5,6.,5.8));
#9686=CARTESIAN_POINT('',(13.5,6.,1.6));
#9687=CARTESIAN_POINT('',(16.5,6.,5.8));
#9688=CARTESIAN_POINT('',(16.5,6.,5.8));
#9689=CARTESIAN_POINT('',(16.5,6.,1.6));
#9690=CARTESIAN_POINT('Origin',(16.5,-6.,1.6));
#9691=CARTESIAN_POINT('',(16.5,-6.,1.6));
#9692=CARTESIAN_POINT('',(16.5,-6.,1.6));
#9693=CARTESIAN_POINT('',(16.5,-6.,5.8));
#9694=CARTESIAN_POINT('',(16.5,-6.,5.8));
#9695=CARTESIAN_POINT('',(16.5,-6.,1.6));
#9696=CARTESIAN_POINT('Origin',(13.5,-6.,1.6));
#9697=CARTESIAN_POINT('',(13.5,-6.,1.6));
#9698=CARTESIAN_POINT('',(13.5,-6.,1.6));
#9699=CARTESIAN_POINT('',(13.5,-6.,5.8));
#9700=CARTESIAN_POINT('',(13.5,-6.,5.8));
#9701=CARTESIAN_POINT('',(13.5,-6.,1.6));
#9702=CARTESIAN_POINT('Origin',(13.5,6.,1.6));
#9703=CARTESIAN_POINT('',(13.5,6.,1.6));
#9704=CARTESIAN_POINT('',(13.5,6.,5.8));
#9705=CARTESIAN_POINT('Origin',(15.,0.,5.8));
#9706=CARTESIAN_POINT('Origin',(15.,0.,1.6));
#9707=CARTESIAN_POINT('',(0.,0.,0.));
#9708=CARTESIAN_POINT('Origin',(15.,0.,5.7));
#9709=CARTESIAN_POINT('',(14.75,-3.06161699786838E-17,5.8));
#9710=CARTESIAN_POINT('Origin',(15.,0.,5.8));
#9711=CARTESIAN_POINT('',(14.75,3.06161699786838E-17,6.6));
#9712=CARTESIAN_POINT('',(14.75,-3.06161699786838E-17,5.7));
#9713=CARTESIAN_POINT('Origin',(15.,0.,6.6));
#9714=CARTESIAN_POINT('Origin',(16.,-2.2,5.7));
#9715=CARTESIAN_POINT('',(15.725,-2.2,5.8));
#9716=CARTESIAN_POINT('Origin',(16.,-2.2,5.8));
#9717=CARTESIAN_POINT('',(15.725,-2.2,6.6));
#9718=CARTESIAN_POINT('',(15.725,-2.2,5.7));
#9719=CARTESIAN_POINT('Origin',(16.,-2.2,6.6));
#9720=CARTESIAN_POINT('Origin',(14.,2.2,5.7));
#9721=CARTESIAN_POINT('',(13.725,2.2,5.8));
#9722=CARTESIAN_POINT('Origin',(14.,2.2,5.8));
#9723=CARTESIAN_POINT('',(13.725,2.2,6.6));
#9724=CARTESIAN_POINT('',(13.725,2.2,5.7));
#9725=CARTESIAN_POINT('Origin',(14.,2.2,6.6));
#9726=CARTESIAN_POINT('Origin',(14.,-2.2,5.7));
#9727=CARTESIAN_POINT('',(13.725,-2.2,5.8));
#9728=CARTESIAN_POINT('Origin',(14.,-2.2,5.8));
#9729=CARTESIAN_POINT('',(13.725,-2.2,6.6));
#9730=CARTESIAN_POINT('',(13.725,-2.2,5.7));
#9731=CARTESIAN_POINT('Origin',(14.,-2.2,6.6));
#9732=CARTESIAN_POINT('Origin',(16.,2.2,5.7));
#9733=CARTESIAN_POINT('',(15.725,2.2,5.8));
#9734=CARTESIAN_POINT('Origin',(16.,2.2,5.8));
#9735=CARTESIAN_POINT('',(15.725,2.2,6.6));
#9736=CARTESIAN_POINT('',(15.725,2.2,5.7));
#9737=CARTESIAN_POINT('Origin',(16.,2.2,6.6));
#9738=CARTESIAN_POINT('Origin',(18.,6.5,5.8));
#9739=CARTESIAN_POINT('',(18.,6.5,5.8));
#9740=CARTESIAN_POINT('',(12.,6.5,5.8));
#9741=CARTESIAN_POINT('',(18.,6.5,5.8));
#9742=CARTESIAN_POINT('',(12.,6.5,6.6));
#9743=CARTESIAN_POINT('',(12.,6.5,5.8));
#9744=CARTESIAN_POINT('',(18.,6.5,6.6));
#9745=CARTESIAN_POINT('',(18.,6.5,6.6));
#9746=CARTESIAN_POINT('',(18.,6.5,5.8));
#9747=CARTESIAN_POINT('Origin',(18.,-6.5,5.8));
#9748=CARTESIAN_POINT('',(18.,-6.5,5.8));
#9749=CARTESIAN_POINT('',(18.,-6.5,5.8));
#9750=CARTESIAN_POINT('',(18.,-6.5,6.6));
#9751=CARTESIAN_POINT('',(18.,-6.5,6.6));
#9752=CARTESIAN_POINT('',(18.,-6.5,5.8));
#9753=CARTESIAN_POINT('Origin',(12.,-6.5,5.8));
#9754=CARTESIAN_POINT('',(12.,-6.5,5.8));
#9755=CARTESIAN_POINT('',(12.,-6.5,5.8));
#9756=CARTESIAN_POINT('',(12.,-6.5,6.6));
#9757=CARTESIAN_POINT('',(12.,-6.5,6.6));
#9758=CARTESIAN_POINT('',(12.,-6.5,5.8));
#9759=CARTESIAN_POINT('Origin',(12.,6.5,5.8));
#9760=CARTESIAN_POINT('',(12.,6.5,5.8));
#9761=CARTESIAN_POINT('',(12.,6.5,6.6));
#9762=CARTESIAN_POINT('Origin',(15.,0.,6.6));
#9763=CARTESIAN_POINT('Origin',(15.,0.,5.8));
#9764=CARTESIAN_POINT('',(0.,0.,0.));
#9765=CARTESIAN_POINT('',(0.,0.,0.));
#9766=CARTESIAN_POINT('Origin',(0.75,1.2,0.));
#9767=CARTESIAN_POINT('',(0.885663593019381,1.2,-0.16));
#9768=CARTESIAN_POINT('',(0.885663593019381,1.2,0.16));
#9769=CARTESIAN_POINT('Origin',(0.,1.2,0.));
#9770=CARTESIAN_POINT('',(0.93,1.2,-0.16));
#9771=CARTESIAN_POINT('',(0.93,1.2,-0.16));
#9772=CARTESIAN_POINT('',(0.93,1.2,0.16));
#9773=CARTESIAN_POINT('',(0.93,1.2,0.16));
#9774=CARTESIAN_POINT('',(0.57,1.2,0.16));
#9775=CARTESIAN_POINT('Origin',(0.57,0.,0.16));
#9776=CARTESIAN_POINT('',(0.885663593019381,-1.2,0.16));
#9777=CARTESIAN_POINT('',(0.885663593019381,0.,0.16));
#9778=CARTESIAN_POINT('',(0.93,-1.2,0.16));
#9779=CARTESIAN_POINT('',(0.93,0.,0.16));
#9780=CARTESIAN_POINT('',(0.57,-1.2,0.16));
#9781=CARTESIAN_POINT('Origin',(0.75,-1.2,0.));
#9782=CARTESIAN_POINT('',(0.885663593019381,-1.2,-0.16));
#9783=CARTESIAN_POINT('Origin',(0.,-1.2,0.));
#9784=CARTESIAN_POINT('',(0.93,-1.2,-0.16));
#9785=CARTESIAN_POINT('',(0.93,-1.2,0.16));
#9786=CARTESIAN_POINT('',(0.93,-1.2,-0.16));
#9787=CARTESIAN_POINT('Origin',(0.93,0.,-0.16));
#9788=CARTESIAN_POINT('',(0.885663593019381,0.,-0.16));
#9789=CARTESIAN_POINT('',(0.93,0.,-0.16));
#9790=CARTESIAN_POINT('Origin',(0.93,0.,0.16));
#9791=CARTESIAN_POINT('Origin',(1.05,1.5,0.));
#9792=CARTESIAN_POINT('',(-1.05,1.5,-1.28587913910472E-16));
#9793=CARTESIAN_POINT('Origin',(0.,1.5,0.));
#9794=CARTESIAN_POINT('',(-0.9,1.5,-1.10218211923262E-16));
#9795=CARTESIAN_POINT('Origin',(0.,1.5,0.));
#9796=CARTESIAN_POINT('Origin',(0.,1.315,0.));
#9797=CARTESIAN_POINT('',(-1.05,1.13,-1.28587913910472E-16));
#9798=CARTESIAN_POINT('Origin',(0.,1.13,0.));
#9799=CARTESIAN_POINT('',(-1.05,1.315,-1.28587913910472E-16));
#9800=CARTESIAN_POINT('Origin',(1.,1.13,0.));
#9801=CARTESIAN_POINT('',(-1.,1.13,-1.22464679914735E-16));
#9802=CARTESIAN_POINT('Origin',(0.,1.13,0.));
#9803=CARTESIAN_POINT('Origin',(0.,1.065,0.));
#9804=CARTESIAN_POINT('',(-1.,1.,-1.22464679914735E-16));
#9805=CARTESIAN_POINT('Origin',(0.,1.,0.));
#9806=CARTESIAN_POINT('',(-1.,1.065,-1.22464679914735E-16));
#9807=CARTESIAN_POINT('Origin',(1.05,1.,0.));
#9808=CARTESIAN_POINT('',(-1.05,1.,-1.28587913910472E-16));
#9809=CARTESIAN_POINT('Origin',(0.,1.,0.));
#9810=CARTESIAN_POINT('Origin',(0.,0.,0.));
#9811=CARTESIAN_POINT('',(-1.05,-1.,-1.28587913910472E-16));
#9812=CARTESIAN_POINT('Origin',(0.,-1.,0.));
#9813=CARTESIAN_POINT('',(-1.05,0.,-1.28587913910472E-16));
#9814=CARTESIAN_POINT('Origin',(1.,-1.,0.));
#9815=CARTESIAN_POINT('',(-1.,-1.,-1.22464679914735E-16));
#9816=CARTESIAN_POINT('Origin',(0.,-1.,0.));
#9817=CARTESIAN_POINT('Origin',(0.,-1.065,0.));
#9818=CARTESIAN_POINT('',(-1.,-1.13,-1.22464679914735E-16));
#9819=CARTESIAN_POINT('Origin',(0.,-1.13,0.));
#9820=CARTESIAN_POINT('',(-1.,-1.065,-1.22464679914735E-16));
#9821=CARTESIAN_POINT('Origin',(1.05,-1.13,0.));
#9822=CARTESIAN_POINT('',(-1.05,-1.13,-1.28587913910472E-16));
#9823=CARTESIAN_POINT('Origin',(0.,-1.13,0.));
#9824=CARTESIAN_POINT('Origin',(0.,-1.315,0.));
#9825=CARTESIAN_POINT('',(-1.05,-1.5,-1.28587913910472E-16));
#9826=CARTESIAN_POINT('Origin',(0.,-1.5,0.));
#9827=CARTESIAN_POINT('',(-1.05,-1.315,-1.28587913910472E-16));
#9828=CARTESIAN_POINT('Origin',(0.9,-1.5,0.));
#9829=CARTESIAN_POINT('',(-0.9,-1.5,-1.10218211923262E-16));
#9830=CARTESIAN_POINT('Origin',(0.,-1.5,0.));
#9831=CARTESIAN_POINT('Origin',(0.,0.,0.));
#9832=CARTESIAN_POINT('',(-0.9,0.,-1.10218211923262E-16));
#9833=CARTESIAN_POINT('',(0.,0.,0.));
#9834=CARTESIAN_POINT('Origin',(0.75,1.2,0.));
#9835=CARTESIAN_POINT('',(0.880582193778639,1.2,0.16));
#9836=CARTESIAN_POINT('',(0.880582193778639,1.2,-0.16));
#9837=CARTESIAN_POINT('Origin',(0.,1.2,0.));
#9838=CARTESIAN_POINT('',(0.583459510163302,1.2,0.16));
#9839=CARTESIAN_POINT('',(0.57,1.2,0.16));
#9840=CARTESIAN_POINT('',(0.583459510163302,1.2,-0.16));
#9841=CARTESIAN_POINT('Origin',(0.,1.2,0.));
#9842=CARTESIAN_POINT('',(0.93,1.2,-0.16));
#9843=CARTESIAN_POINT('Origin',(0.93,0.,-0.16));
#9844=CARTESIAN_POINT('',(0.880582193778639,-1.2,-0.16));
#9845=CARTESIAN_POINT('',(0.880582193778639,0.,-0.16));
#9846=CARTESIAN_POINT('',(0.583459510163302,-1.2,-0.16));
#9847=CARTESIAN_POINT('',(0.583459510163302,0.,-0.16));
#9848=CARTESIAN_POINT('',(0.93,-1.2,-0.16));
#9849=CARTESIAN_POINT('Origin',(0.75,-1.2,0.));
#9850=CARTESIAN_POINT('',(0.880582193778639,-1.2,0.16));
#9851=CARTESIAN_POINT('Origin',(0.,-1.2,0.));
#9852=CARTESIAN_POINT('',(0.583459510163302,-1.2,0.16));
#9853=CARTESIAN_POINT('Origin',(0.,-1.2,0.));
#9854=CARTESIAN_POINT('',(0.57,-1.2,0.16));
#9855=CARTESIAN_POINT('Origin',(0.57,0.,0.16));
#9856=CARTESIAN_POINT('',(0.880582193778639,0.,0.16));
#9857=CARTESIAN_POINT('',(0.583459510163302,0.,0.16));
#9858=CARTESIAN_POINT('Origin',(0.895,1.35,0.));
#9859=CARTESIAN_POINT('',(-0.895,1.35,-1.09605888523688E-16));
#9860=CARTESIAN_POINT('Origin',(0.,1.35,0.));
#9861=CARTESIAN_POINT('',(-0.605,1.35,-7.40911313484149E-17));
#9862=CARTESIAN_POINT('Origin',(0.,1.35,0.));
#9863=CARTESIAN_POINT('Origin',(0.,0.,0.));
#9864=CARTESIAN_POINT('',(-0.895,-1.35,-1.09605888523688E-16));
#9865=CARTESIAN_POINT('Origin',(0.,-1.35,0.));
#9866=CARTESIAN_POINT('',(-0.895,0.,-1.09605888523688E-16));
#9867=CARTESIAN_POINT('Origin',(0.605,-1.35,0.));
#9868=CARTESIAN_POINT('',(-0.605,-1.35,-7.40911313484149E-17));
#9869=CARTESIAN_POINT('Origin',(0.,-1.35,0.));
#9870=CARTESIAN_POINT('Origin',(0.,0.,0.));
#9871=CARTESIAN_POINT('',(-0.605,0.,-7.40911313484149E-17));
#9872=CARTESIAN_POINT('',(0.,0.,0.));
#9873=CARTESIAN_POINT('',(0.,0.,0.));
#9874=CARTESIAN_POINT('',(0.,0.,0.));
#9875=CARTESIAN_POINT('Origin',(9.9,5.5,3.));
#9876=CARTESIAN_POINT('',(10.,5.5,3.225));
#9877=CARTESIAN_POINT('Origin',(10.,5.5,3.));
#9878=CARTESIAN_POINT('',(10.5,5.5,3.225));
#9879=CARTESIAN_POINT('',(9.9,5.5,3.225));
#9880=CARTESIAN_POINT('Origin',(10.5,5.5,3.));
#9881=CARTESIAN_POINT('Origin',(9.9,-5.5,5.));
#9882=CARTESIAN_POINT('',(10.,-5.5,5.225));
#9883=CARTESIAN_POINT('Origin',(10.,-5.5,5.));
#9884=CARTESIAN_POINT('',(10.5,-5.5,5.225));
#9885=CARTESIAN_POINT('',(9.9,-5.5,5.225));
#9886=CARTESIAN_POINT('Origin',(10.5,-5.5,5.));
#9887=CARTESIAN_POINT('Origin',(9.9,-5.5,3.));
#9888=CARTESIAN_POINT('',(10.,-5.5,3.225));
#9889=CARTESIAN_POINT('Origin',(10.,-5.5,3.));
#9890=CARTESIAN_POINT('',(10.5,-5.5,3.225));
#9891=CARTESIAN_POINT('',(9.9,-5.5,3.225));
#9892=CARTESIAN_POINT('Origin',(10.5,-5.5,3.));
#9893=CARTESIAN_POINT('Origin',(9.9,5.5,5.));
#9894=CARTESIAN_POINT('',(10.,5.5,5.225));
#9895=CARTESIAN_POINT('Origin',(10.,5.5,5.));
#9896=CARTESIAN_POINT('',(10.5,5.5,5.225));
#9897=CARTESIAN_POINT('',(9.9,5.5,5.225));
#9898=CARTESIAN_POINT('Origin',(10.5,5.5,5.));
#9899=CARTESIAN_POINT('Origin',(9.9,-4.,3.3));
#9900=CARTESIAN_POINT('',(10.,-4.,4.));
#9901=CARTESIAN_POINT('Origin',(10.,-4.,3.3));
#9902=CARTESIAN_POINT('',(10.5,-4.,4.));
#9903=CARTESIAN_POINT('',(9.9,-4.,4.));
#9904=CARTESIAN_POINT('Origin',(10.5,-4.,3.3));
#9905=CARTESIAN_POINT('Origin',(9.9,4.,3.3));
#9906=CARTESIAN_POINT('',(10.,4.,4.));
#9907=CARTESIAN_POINT('Origin',(10.,4.,3.3));
#9908=CARTESIAN_POINT('',(10.5,4.,4.));
#9909=CARTESIAN_POINT('',(9.9,4.,4.));
#9910=CARTESIAN_POINT('Origin',(10.5,4.,3.3));
#9911=CARTESIAN_POINT('Origin',(10.5,6.,1.6));
#9912=CARTESIAN_POINT('',(10.5,6.,1.6));
#9913=CARTESIAN_POINT('',(10.,6.,1.6));
#9914=CARTESIAN_POINT('',(10.5,6.,1.6));
#9915=CARTESIAN_POINT('',(10.,6.,5.8));
#9916=CARTESIAN_POINT('',(10.,6.,1.6));
#9917=CARTESIAN_POINT('',(10.5,6.,5.8));
#9918=CARTESIAN_POINT('',(10.5,6.,5.8));
#9919=CARTESIAN_POINT('',(10.5,6.,1.6));
#9920=CARTESIAN_POINT('Origin',(10.5,-6.,1.6));
#9921=CARTESIAN_POINT('',(10.5,-6.,1.6));
#9922=CARTESIAN_POINT('',(10.5,-6.,1.6));
#9923=CARTESIAN_POINT('',(10.5,-6.,5.8));
#9924=CARTESIAN_POINT('',(10.5,-6.,5.8));
#9925=CARTESIAN_POINT('',(10.5,-6.,1.6));
#9926=CARTESIAN_POINT('Origin',(10.,-6.,1.6));
#9927=CARTESIAN_POINT('',(10.,-6.,1.6));
#9928=CARTESIAN_POINT('',(10.,-6.,1.6));
#9929=CARTESIAN_POINT('',(10.,-6.,5.8));
#9930=CARTESIAN_POINT('',(10.,-6.,5.8));
#9931=CARTESIAN_POINT('',(10.,-6.,1.6));
#9932=CARTESIAN_POINT('Origin',(10.,6.,1.6));
#9933=CARTESIAN_POINT('',(10.,6.,1.6));
#9934=CARTESIAN_POINT('',(10.,6.,5.8));
#9935=CARTESIAN_POINT('Origin',(10.25,0.,5.8));
#9936=CARTESIAN_POINT('Origin',(10.25,0.,1.6));
#9937=CARTESIAN_POINT('',(0.,0.,0.));
#9938=CARTESIAN_POINT('Origin',(0.3,0.4,0.));
#9939=CARTESIAN_POINT('',(-0.3,0.4,-3.67394039744206E-17));
#9940=CARTESIAN_POINT('Origin',(0.,0.4,0.));
#9941=CARTESIAN_POINT('Origin',(0.,0.375,0.));
#9942=CARTESIAN_POINT('',(-0.35,0.35,-4.28626379701573E-17));
#9943=CARTESIAN_POINT('Origin',(0.,0.35,0.));
#9944=CARTESIAN_POINT('',(-0.325,0.375,-3.9801020972289E-17));
#9945=CARTESIAN_POINT('Origin',(0.,0.19,0.));
#9946=CARTESIAN_POINT('',(-0.35,0.03,-4.28626379701574E-17));
#9947=CARTESIAN_POINT('Origin',(0.,0.03,0.));
#9948=CARTESIAN_POINT('',(-0.35,0.19,-4.28626379701574E-17));
#9949=CARTESIAN_POINT('Origin',(0.,0.0149999999999999,0.));
#9950=CARTESIAN_POINT('',(-0.32,-3.29597460435593E-17,-3.91886975727153E-17));
#9951=CARTESIAN_POINT('Origin',(0.,0.,0.));
#9952=CARTESIAN_POINT('',(-0.335,0.0149999999999999,-4.10256677714363E-17));
#9953=CARTESIAN_POINT('Origin',(0.22,0.,0.));
#9954=CARTESIAN_POINT('',(-0.22,-6.93889390390723E-18,-2.69422295812418E-17));
#9955=CARTESIAN_POINT('Origin',(0.,0.,0.));
#9956=CARTESIAN_POINT('Origin',(0.,-0.02,0.));
#9957=CARTESIAN_POINT('',(-0.1954,-0.0492,2.39295984553393E-17));
#9958=CARTESIAN_POINT('Origin',(0.,-0.0492,0.));
#9959=CARTESIAN_POINT('',(-0.21,-0.02,-2.57175827820944E-17));
#9960=CARTESIAN_POINT('Origin',(0.,-0.8,0.));
#9961=CARTESIAN_POINT('',(-0.1954,-1.5646,2.39295984553393E-17));
#9962=CARTESIAN_POINT('Origin',(0.,-1.5646,0.));
#9963=CARTESIAN_POINT('',(-0.1954,-0.8,-2.39295984553393E-17));
#9964=CARTESIAN_POINT('Origin',(0.,-1.58,0.));
#9965=CARTESIAN_POINT('',(-0.16,-1.6,-1.95943487863577E-17));
#9966=CARTESIAN_POINT('Origin',(0.,-1.6,0.));
#9967=CARTESIAN_POINT('',(-0.18,-1.58,-2.20436423846524E-17));
#9968=CARTESIAN_POINT('Origin',(0.,-1.6,0.));
#9969=CARTESIAN_POINT('Origin',(0.0866025403784439,-0.4,-0.15));
#9970=CARTESIAN_POINT('',(0.173205080756888,-0.4,0.));
#9971=CARTESIAN_POINT('',(0.0866025403784439,-0.4,-0.15));
#9972=CARTESIAN_POINT('',(0.173205080756888,-0.4,0.));
#9973=CARTESIAN_POINT('',(0.0866025403784439,-0.64,-0.15));
#9974=CARTESIAN_POINT('',(0.0866025403784439,-0.4,-0.15));
#9975=CARTESIAN_POINT('',(0.173205080756888,-0.64,0.));
#9976=CARTESIAN_POINT('',(0.173205080756888,-0.64,0.));
#9977=CARTESIAN_POINT('',(0.173205080756888,-0.4,0.));
#9978=CARTESIAN_POINT('Origin',(-0.0866025403784438,-0.4,-0.15));
#9979=CARTESIAN_POINT('',(-0.0866025403784438,-0.4,-0.15));
#9980=CARTESIAN_POINT('',(0.0866025403784439,-0.4,-0.15));
#9981=CARTESIAN_POINT('',(-0.0866025403784438,-0.64,-0.15));
#9982=CARTESIAN_POINT('',(-0.0866025403784438,-0.4,-0.15));
#9983=CARTESIAN_POINT('',(0.0866025403784439,-0.64,-0.15));
#9984=CARTESIAN_POINT('Origin',(-0.173205080756888,-0.4,-2.77555756156289E-17));
#9985=CARTESIAN_POINT('',(-0.173205080756888,-0.4,-2.12115047744981E-17));
#9986=CARTESIAN_POINT('',(-0.0866025403784438,-0.4,-0.15));
#9987=CARTESIAN_POINT('',(-0.173205080756888,-0.64,-2.77555756156289E-17));
#9988=CARTESIAN_POINT('',(-0.173205080756888,-0.4,-2.12115047744981E-17));
#9989=CARTESIAN_POINT('',(-0.0866025403784438,-0.64,-0.15));
#9990=CARTESIAN_POINT('Origin',(-0.0866025403784439,-0.4,0.15));
#9991=CARTESIAN_POINT('',(-0.0866025403784439,-0.4,0.15));
#9992=CARTESIAN_POINT('',(-0.173205080756888,-0.4,-2.12115047744981E-17));
#9993=CARTESIAN_POINT('',(-0.0866025403784439,-0.64,0.15));
#9994=CARTESIAN_POINT('',(-0.0866025403784439,-0.4,0.15));
#9995=CARTESIAN_POINT('',(-0.173205080756888,-0.64,-2.12115047744981E-17));
#9996=CARTESIAN_POINT('Origin',(0.0866025403784439,-0.4,0.15));
#9997=CARTESIAN_POINT('',(0.0866025403784439,-0.4,0.15));
#9998=CARTESIAN_POINT('',(-0.0866025403784439,-0.4,0.15));
#9999=CARTESIAN_POINT('',(0.0866025403784439,-0.64,0.15));
#10000=CARTESIAN_POINT('',(0.0866025403784439,-0.4,0.15));
#10001=CARTESIAN_POINT('',(-0.0866025403784439,-0.64,0.15));
#10002=CARTESIAN_POINT('Origin',(0.173205080756888,-0.4,0.));
#10003=CARTESIAN_POINT('',(0.0866025403784439,-0.4,0.15));
#10004=CARTESIAN_POINT('',(0.0866025403784439,-0.64,0.15));
#10005=CARTESIAN_POINT('Origin',(0.,-0.4,-2.77555756156289E-17));
#10006=CARTESIAN_POINT('Origin',(0.,-0.64,-2.77555756156289E-17));
#10007=CARTESIAN_POINT('',(0.,0.,0.));
#10008=CARTESIAN_POINT('Origin',(0.375,0.5,0.));
#10009=CARTESIAN_POINT('',(-0.375,0.5,-4.59242549680257E-17));
#10010=CARTESIAN_POINT('Origin',(0.,0.5,0.));
#10011=CARTESIAN_POINT('Origin',(0.,0.475,0.));
#10012=CARTESIAN_POINT('',(-0.425,0.45,-5.20474889637625E-17));
#10013=CARTESIAN_POINT('Origin',(0.,0.45,0.));
#10014=CARTESIAN_POINT('',(-0.4,0.475,-4.89858719658941E-17));
#10015=CARTESIAN_POINT('Origin',(0.,0.24,0.));
#10016=CARTESIAN_POINT('',(-0.425,0.0299999999999998,-5.20474889637625E-17));
#10017=CARTESIAN_POINT('Origin',(0.,0.0299999999999998,0.));
#10018=CARTESIAN_POINT('',(-0.425,0.24,-5.20474889637625E-17));
#10019=CARTESIAN_POINT('Origin',(0.,0.0150000000000001,0.));
#10020=CARTESIAN_POINT('',(-0.395,4.85722573273506E-17,-4.83735485663204E-17));
#10021=CARTESIAN_POINT('Origin',(0.,0.,0.));
#10022=CARTESIAN_POINT('',(-0.41,0.0150000000000001,-5.02105187650415E-17));
#10023=CARTESIAN_POINT('Origin',(0.27,0.,0.));
#10024=CARTESIAN_POINT('',(-0.27,0.,-3.30654635769785E-17));
#10025=CARTESIAN_POINT('Origin',(0.,0.,0.));
#10026=CARTESIAN_POINT('Origin',(0.,-0.02,0.));
#10027=CARTESIAN_POINT('',(-0.24505,-0.0498999999999999,3.00099698131059E-17));
#10028=CARTESIAN_POINT('Origin',(0.,-0.0498999999999999,0.));
#10029=CARTESIAN_POINT('',(-0.26,-0.02,-3.18408167778312E-17));
#10030=CARTESIAN_POINT('Origin',(0.,-0.995,0.));
#10031=CARTESIAN_POINT('',(-0.24505,-1.95495,3.00099698131059E-17));
#10032=CARTESIAN_POINT('Origin',(0.,-1.95495,0.));
#10033=CARTESIAN_POINT('',(-0.24505,-0.995,-3.00099698131059E-17));
#10034=CARTESIAN_POINT('Origin',(0.,-1.975,0.));
#10035=CARTESIAN_POINT('',(-0.2,-2.,-2.44929359829471E-17));
#10036=CARTESIAN_POINT('Origin',(0.,-2.,0.));
#10037=CARTESIAN_POINT('',(-0.225,-1.975,-2.75545529808154E-17));
#10038=CARTESIAN_POINT('Origin',(0.,-2.,0.));
#10039=CARTESIAN_POINT('Origin',(0.115470053837925,-0.5,-0.2));
#10040=CARTESIAN_POINT('',(0.23094010767585,-0.5,0.));
#10041=CARTESIAN_POINT('',(0.115470053837925,-0.5,-0.2));
#10042=CARTESIAN_POINT('',(0.23094010767585,-0.5,0.));
#10043=CARTESIAN_POINT('',(0.115470053837925,-0.8,-0.2));
#10044=CARTESIAN_POINT('',(0.115470053837925,-0.5,-0.2));
#10045=CARTESIAN_POINT('',(0.23094010767585,-0.8,0.));
#10046=CARTESIAN_POINT('',(0.23094010767585,-0.8,0.));
#10047=CARTESIAN_POINT('',(0.23094010767585,-0.5,0.));
#10048=CARTESIAN_POINT('Origin',(-0.115470053837925,-0.5,-0.2));
#10049=CARTESIAN_POINT('',(-0.115470053837925,-0.5,-0.2));
#10050=CARTESIAN_POINT('',(0.115470053837925,-0.5,-0.2));
#10051=CARTESIAN_POINT('',(-0.115470053837925,-0.8,-0.2));
#10052=CARTESIAN_POINT('',(-0.115470053837925,-0.5,-0.2));
#10053=CARTESIAN_POINT('',(0.115470053837925,-0.8,-0.2));
#10054=CARTESIAN_POINT('Origin',(-0.23094010767585,-0.5,-2.77555756156289E-17));
#10055=CARTESIAN_POINT('',(-0.23094010767585,-0.5,-2.82820063659975E-17));
#10056=CARTESIAN_POINT('',(-0.115470053837925,-0.5,-0.2));
#10057=CARTESIAN_POINT('',(-0.23094010767585,-0.8,-2.77555756156289E-17));
#10058=CARTESIAN_POINT('',(-0.23094010767585,-0.5,-2.82820063659975E-17));
#10059=CARTESIAN_POINT('',(-0.115470053837925,-0.8,-0.2));
#10060=CARTESIAN_POINT('Origin',(-0.115470053837925,-0.5,0.2));
#10061=CARTESIAN_POINT('',(-0.115470053837925,-0.5,0.2));
#10062=CARTESIAN_POINT('',(-0.23094010767585,-0.5,-2.82820063659975E-17));
#10063=CARTESIAN_POINT('',(-0.115470053837925,-0.8,0.2));
#10064=CARTESIAN_POINT('',(-0.115470053837925,-0.5,0.2));
#10065=CARTESIAN_POINT('',(-0.23094010767585,-0.8,-2.82820063659975E-17));
#10066=CARTESIAN_POINT('Origin',(0.115470053837925,-0.5,0.2));
#10067=CARTESIAN_POINT('',(0.115470053837925,-0.5,0.2));
#10068=CARTESIAN_POINT('',(-0.115470053837925,-0.5,0.2));
#10069=CARTESIAN_POINT('',(0.115470053837925,-0.8,0.2));
#10070=CARTESIAN_POINT('',(0.115470053837925,-0.5,0.2));
#10071=CARTESIAN_POINT('',(-0.115470053837925,-0.8,0.2));
#10072=CARTESIAN_POINT('Origin',(0.23094010767585,-0.5,0.));
#10073=CARTESIAN_POINT('',(0.115470053837925,-0.5,0.2));
#10074=CARTESIAN_POINT('',(0.115470053837925,-0.8,0.2));
#10075=CARTESIAN_POINT('Origin',(0.,-0.5,0.));
#10076=CARTESIAN_POINT('Origin',(0.,-0.8,0.));
#10077=CARTESIAN_POINT('',(0.,0.,0.));
#10078=CARTESIAN_POINT('',(0.,-4.,3.3));
#10079=CARTESIAN_POINT('',(1.,-4.,1.));
#10080=CARTESIAN_POINT('',(1.,-5.6,1.6));
#10081=CARTESIAN_POINT('',(1.,-2.4,1.6));
#10082=CARTESIAN_POINT('',(1.,-5.2,4.35));
#10083=CARTESIAN_POINT('',(29.,-4.,1.));
#10084=CARTESIAN_POINT('',(29.,-5.6,1.6));
#10085=CARTESIAN_POINT('',(29.,-2.4,1.6));
#10086=CARTESIAN_POINT('',(29.,-5.2,4.35));
#10087=CARTESIAN_POINT('',(0.,4.,3.3));
#10088=CARTESIAN_POINT('',(1.,4.,1.));
#10089=CARTESIAN_POINT('',(1.,2.4,1.6));
#10090=CARTESIAN_POINT('',(1.,5.6,1.6));
#10091=CARTESIAN_POINT('',(1.,2.8,4.35));
#10092=CARTESIAN_POINT('',(29.,4.,1.));
#10093=CARTESIAN_POINT('',(29.,2.4,1.6));
#10094=CARTESIAN_POINT('',(29.,5.6,1.6));
#10095=CARTESIAN_POINT('',(29.,2.8,4.35));
#10096=CARTESIAN_POINT('',(0.,0.,0.));
#10097=CARTESIAN_POINT('',(3.5,-5.5,2.));
#10098=CARTESIAN_POINT('',(3.5,5.5,2.));
#10099=CARTESIAN_POINT('',(23.,0.,0.));
#10100=CARTESIAN_POINT('',(26.5,-5.5,2.));
#10101=CARTESIAN_POINT('',(26.5,5.5,2.));
#10102=CARTESIAN_POINT('',(0.,0.,0.));
#10103=CARTESIAN_POINT('',(21.8,0.,0.));
#10104=CARTESIAN_POINT('',(0.,0.,0.));
#10105=CARTESIAN_POINT('',(9.5,-1.6,1.8));
#10106=CARTESIAN_POINT('',(9.5,1.6,1.8));
#10107=CARTESIAN_POINT('',(11.7,-1.6,1.8));
#10108=CARTESIAN_POINT('',(11.7,1.6,1.8));
#10109=CARTESIAN_POINT('',(9.,0.,3.3));
#10110=CARTESIAN_POINT('',(9.52,0.,3.3));
#10111=CARTESIAN_POINT('',(17.124861099224,4.,3.3));
#10112=CARTESIAN_POINT('',(18.1,4.,-6.7));
#10113=CARTESIAN_POINT('',(23.4,4.,4.7));
#10114=CARTESIAN_POINT('',(0.,0.,0.));
#10115=CARTESIAN_POINT('Origin',(15.,0.,6.6));
#10116=CARTESIAN_POINT('',(14.67,-4.04133443718627E-17,8.2));
#10117=CARTESIAN_POINT('Origin',(15.,0.,8.2));
#10118=CARTESIAN_POINT('',(14.67,-4.04133443718627E-17,6.6));
#10119=CARTESIAN_POINT('',(14.67,-4.04133443718627E-17,6.6));
#10120=CARTESIAN_POINT('Origin',(15.,0.,6.6));
#10121=CARTESIAN_POINT('Origin',(15.,0.,6.6));
#10122=CARTESIAN_POINT('',(13.5,-1.83697019872103E-16,8.2));
#10123=CARTESIAN_POINT('Origin',(15.,0.,8.2));
#10124=CARTESIAN_POINT('',(13.5,-1.83697019872103E-16,6.6));
#10125=CARTESIAN_POINT('',(13.5,-1.83697019872103E-16,6.6));
#10126=CARTESIAN_POINT('Origin',(15.,0.,6.6));
#10127=CARTESIAN_POINT('Origin',(15.,0.,8.2));
#10128=CARTESIAN_POINT('Origin',(15.,0.,6.6));
#10129=CARTESIAN_POINT('',(0.,0.,0.));
#10130=CARTESIAN_POINT('Origin',(0.,0.,0.));
#10131=CARTESIAN_POINT('',(-0.32,0.16,3.91886975727153E-17));
#10132=CARTESIAN_POINT('Origin',(0.,0.16,0.));
#10133=CARTESIAN_POINT('',(-0.32,0.,3.91886975727153E-17));
#10134=CARTESIAN_POINT('',(-0.32,0.,3.91886975727153E-17));
#10135=CARTESIAN_POINT('Origin',(0.,0.,0.));
#10136=CARTESIAN_POINT('Origin',(0.,0.,0.));
#10137=CARTESIAN_POINT('',(-0.6,0.16,7.34788079488412E-17));
#10138=CARTESIAN_POINT('Origin',(0.,0.16,0.));
#10139=CARTESIAN_POINT('',(-0.6,0.,7.34788079488412E-17));
#10140=CARTESIAN_POINT('',(-0.6,0.,7.34788079488412E-17));
#10141=CARTESIAN_POINT('Origin',(0.,0.,0.));
#10142=CARTESIAN_POINT('Origin',(0.,0.16,0.));
#10143=CARTESIAN_POINT('Origin',(0.,0.,0.));
#10144=CARTESIAN_POINT('',(0.,0.,0.));
#10145=CARTESIAN_POINT('Origin',(0.45,0.6,0.));
#10146=CARTESIAN_POINT('',(-0.45,0.6,-5.51091059616309E-17));
#10147=CARTESIAN_POINT('Origin',(0.,0.6,0.));
#10148=CARTESIAN_POINT('Origin',(0.,0.575,0.));
#10149=CARTESIAN_POINT('',(-0.5,0.55,-6.12323399573677E-17));
#10150=CARTESIAN_POINT('Origin',(0.,0.55,0.));
#10151=CARTESIAN_POINT('',(-0.475,0.575,-5.81707229594993E-17));
#10152=CARTESIAN_POINT('Origin',(0.,0.29,0.));
#10153=CARTESIAN_POINT('',(-0.5,0.0299999999999998,-6.12323399573677E-17));
#10154=CARTESIAN_POINT('Origin',(0.,0.0299999999999998,0.));
#10155=CARTESIAN_POINT('',(-0.5,0.29,-6.12323399573677E-17));
#10156=CARTESIAN_POINT('Origin',(0.,0.0150000000000001,0.));
#10157=CARTESIAN_POINT('',(-0.47,7.11236625150491E-17,-5.75583995599256E-17));
#10158=CARTESIAN_POINT('Origin',(0.,0.,0.));
#10159=CARTESIAN_POINT('',(-0.485,0.0150000000000001,-5.93953697586466E-17));
#10160=CARTESIAN_POINT('Origin',(0.32,0.,0.));
#10161=CARTESIAN_POINT('',(-0.32,-6.93889390390723E-18,-3.91886975727153E-17));
#10162=CARTESIAN_POINT('Origin',(0.,0.,0.));
#10163=CARTESIAN_POINT('Origin',(0.,-0.02,0.));
#10164=CARTESIAN_POINT('',(-0.2942,-0.0515999999999999,3.60291088309151E-17));
#10165=CARTESIAN_POINT('Origin',(0.,-0.0515999999999999,0.));
#10166=CARTESIAN_POINT('',(-0.31,-0.02,-3.7964050773568E-17));
#10167=CARTESIAN_POINT('Origin',(0.,-1.24,0.));
#10168=CARTESIAN_POINT('',(-0.2942,-2.4458,3.60291088309151E-17));
#10169=CARTESIAN_POINT('Origin',(0.,-2.4458,0.));
#10170=CARTESIAN_POINT('',(-0.2942,-1.24,-3.60291088309151E-17));
#10171=CARTESIAN_POINT('Origin',(0.,-2.47,0.));
#10172=CARTESIAN_POINT('',(-0.24,-2.5,-2.93915231795365E-17));
#10173=CARTESIAN_POINT('Origin',(0.,-2.5,0.));
#10174=CARTESIAN_POINT('',(-0.27,-2.47,-3.30654635769785E-17));
#10175=CARTESIAN_POINT('Origin',(0.,-2.5,0.));
#10176=CARTESIAN_POINT('Origin',(0.144337567297406,-0.6,-0.25));
#10177=CARTESIAN_POINT('',(0.288675134594813,-0.6,0.));
#10178=CARTESIAN_POINT('',(0.144337567297406,-0.6,-0.25));
#10179=CARTESIAN_POINT('',(0.288675134594813,-0.6,0.));
#10180=CARTESIAN_POINT('',(0.144337567297406,-0.96,-0.25));
#10181=CARTESIAN_POINT('',(0.144337567297406,-0.6,-0.25));
#10182=CARTESIAN_POINT('',(0.288675134594813,-0.96,0.));
#10183=CARTESIAN_POINT('',(0.288675134594813,-0.96,0.));
#10184=CARTESIAN_POINT('',(0.288675134594813,-0.6,0.));
#10185=CARTESIAN_POINT('Origin',(-0.144337567297406,-0.6,-0.25));
#10186=CARTESIAN_POINT('',(-0.144337567297406,-0.6,-0.25));
#10187=CARTESIAN_POINT('',(0.144337567297406,-0.6,-0.25));
#10188=CARTESIAN_POINT('',(-0.144337567297406,-0.96,-0.25));
#10189=CARTESIAN_POINT('',(-0.144337567297406,-0.6,-0.25));
#10190=CARTESIAN_POINT('',(0.144337567297406,-0.96,-0.25));
#10191=CARTESIAN_POINT('Origin',(-0.288675134594813,-0.6,-8.32667268468867E-17));
#10192=CARTESIAN_POINT('',(-0.288675134594813,-0.6,-3.53525079574969E-17));
#10193=CARTESIAN_POINT('',(-0.144337567297406,-0.6,-0.25));
#10194=CARTESIAN_POINT('',(-0.288675134594813,-0.96,-5.55111512312578E-17));
#10195=CARTESIAN_POINT('',(-0.288675134594813,-0.6,-3.53525079574969E-17));
#10196=CARTESIAN_POINT('',(-0.144337567297406,-0.96,-0.25));
#10197=CARTESIAN_POINT('Origin',(-0.144337567297407,-0.6,0.25));
#10198=CARTESIAN_POINT('',(-0.144337567297407,-0.6,0.25));
#10199=CARTESIAN_POINT('',(-0.288675134594813,-0.6,-3.53525079574969E-17));
#10200=CARTESIAN_POINT('',(-0.144337567297407,-0.96,0.25));
#10201=CARTESIAN_POINT('',(-0.144337567297407,-0.6,0.25));
#10202=CARTESIAN_POINT('',(-0.288675134594813,-0.96,-3.53525079574969E-17));
#10203=CARTESIAN_POINT('Origin',(0.144337567297406,-0.6,0.25));
#10204=CARTESIAN_POINT('',(0.144337567297406,-0.6,0.25));
#10205=CARTESIAN_POINT('',(-0.144337567297407,-0.6,0.25));
#10206=CARTESIAN_POINT('',(0.144337567297406,-0.96,0.25));
#10207=CARTESIAN_POINT('',(0.144337567297406,-0.6,0.25));
#10208=CARTESIAN_POINT('',(-0.144337567297407,-0.96,0.25));
#10209=CARTESIAN_POINT('Origin',(0.288675134594813,-0.6,0.));
#10210=CARTESIAN_POINT('',(0.144337567297406,-0.6,0.25));
#10211=CARTESIAN_POINT('',(0.144337567297406,-0.96,0.25));
#10212=CARTESIAN_POINT('Origin',(0.,-0.6,0.));
#10213=CARTESIAN_POINT('Origin',(0.,-0.96,0.));
#10214=CARTESIAN_POINT('',(0.,0.,0.));
#10215=CARTESIAN_POINT('',(0.,0.,0.));
#10216=CARTESIAN_POINT('',(15.,-4.,3.3));
#10217=CARTESIAN_POINT('',(15.,4.,3.3));
#10218=CARTESIAN_POINT('',(3.,0.,0.));
#10219=CARTESIAN_POINT('',(6.5,0.,0.));
#10220=CARTESIAN_POINT('',(13.,-5.5,3.));
#10221=CARTESIAN_POINT('',(13.,-5.5,5.));
#10222=CARTESIAN_POINT('',(13.,5.5,3.));
#10223=CARTESIAN_POINT('',(13.,5.5,5.));
#10224=CARTESIAN_POINT('',(17.,-5.5,3.));
#10225=CARTESIAN_POINT('',(17.,-5.5,5.));
#10226=CARTESIAN_POINT('',(17.,5.5,3.));
#10227=CARTESIAN_POINT('',(17.,5.5,5.));
#10228=CARTESIAN_POINT('',(14.,-2.2,6.6));
#10229=CARTESIAN_POINT('',(14.,2.2,6.6));
#10230=CARTESIAN_POINT('',(16.,-2.2,6.6));
#10231=CARTESIAN_POINT('',(16.,2.2,6.6));
#10232=CARTESIAN_POINT('',(0.,0.,0.));
#10233=CARTESIAN_POINT('',(15.,0.,8.2));
#10234=CARTESIAN_POINT('',(15.,0.,8.36));
#10235=CARTESIAN_POINT('',(0.,0.,0.));
#10236=CARTESIAN_POINT('',(0.00173778078960574,1.23259516440783E-32,8.17373283524957E-16));
#10237=UNCERTAINTY_MEASURE_WITH_UNIT(LENGTH_MEASURE(0.001),#10293,
'DISTANCE_ACCURACY_VALUE',
'Maximum model space distance between geometric entities at asserted c
onnectivities');
#10238=UNCERTAINTY_MEASURE_WITH_UNIT(LENGTH_MEASURE(0.001),#10293,
'DISTANCE_ACCURACY_VALUE',
'Maximum model space distance between geometric entities at asserted c
onnectivities');
#10239=UNCERTAINTY_MEASURE_WITH_UNIT(LENGTH_MEASURE(0.001),#10293,
'DISTANCE_ACCURACY_VALUE',
'Maximum model space distance between geometric entities at asserted c
onnectivities');
#10240=UNCERTAINTY_MEASURE_WITH_UNIT(LENGTH_MEASURE(0.001),#10293,
'DISTANCE_ACCURACY_VALUE',
'Maximum model space distance between geometric entities at asserted c
onnectivities');
#10241=UNCERTAINTY_MEASURE_WITH_UNIT(LENGTH_MEASURE(0.001),#10293,
'DISTANCE_ACCURACY_VALUE',
'Maximum model space distance between geometric entities at asserted c
onnectivities');
#10242=UNCERTAINTY_MEASURE_WITH_UNIT(LENGTH_MEASURE(0.001),#10293,
'DISTANCE_ACCURACY_VALUE',
'Maximum model space distance between geometric entities at asserted c
onnectivities');
#10243=UNCERTAINTY_MEASURE_WITH_UNIT(LENGTH_MEASURE(0.001),#10293,
'DISTANCE_ACCURACY_VALUE',
'Maximum model space distance between geometric entities at asserted c
onnectivities');
#10244=UNCERTAINTY_MEASURE_WITH_UNIT(LENGTH_MEASURE(0.001),#10293,
'DISTANCE_ACCURACY_VALUE',
'Maximum model space distance between geometric entities at asserted c
onnectivities');
#10245=UNCERTAINTY_MEASURE_WITH_UNIT(LENGTH_MEASURE(0.001),#10293,
'DISTANCE_ACCURACY_VALUE',
'Maximum model space distance between geometric entities at asserted c
onnectivities');
#10246=UNCERTAINTY_MEASURE_WITH_UNIT(LENGTH_MEASURE(0.001),#10293,
'DISTANCE_ACCURACY_VALUE',
'Maximum model space distance between geometric entities at asserted c
onnectivities');
#10247=UNCERTAINTY_MEASURE_WITH_UNIT(LENGTH_MEASURE(0.001),#10293,
'DISTANCE_ACCURACY_VALUE',
'Maximum model space distance between geometric entities at asserted c
onnectivities');
#10248=UNCERTAINTY_MEASURE_WITH_UNIT(LENGTH_MEASURE(0.001),#10293,
'DISTANCE_ACCURACY_VALUE',
'Maximum model space distance between geometric entities at asserted c
onnectivities');
#10249=UNCERTAINTY_MEASURE_WITH_UNIT(LENGTH_MEASURE(0.001),#10293,
'DISTANCE_ACCURACY_VALUE',
'Maximum model space distance between geometric entities at asserted c
onnectivities');
#10250=UNCERTAINTY_MEASURE_WITH_UNIT(LENGTH_MEASURE(0.001),#10293,
'DISTANCE_ACCURACY_VALUE',
'Maximum model space distance between geometric entities at asserted c
onnectivities');
#10251=UNCERTAINTY_MEASURE_WITH_UNIT(LENGTH_MEASURE(0.001),#10293,
'DISTANCE_ACCURACY_VALUE',
'Maximum model space distance between geometric entities at asserted c
onnectivities');
#10252=UNCERTAINTY_MEASURE_WITH_UNIT(LENGTH_MEASURE(0.001),#10293,
'DISTANCE_ACCURACY_VALUE',
'Maximum model space distance between geometric entities at asserted c
onnectivities');
#10253=UNCERTAINTY_MEASURE_WITH_UNIT(LENGTH_MEASURE(0.001),#10293,
'DISTANCE_ACCURACY_VALUE',
'Maximum model space distance between geometric entities at asserted c
onnectivities');
#10254=UNCERTAINTY_MEASURE_WITH_UNIT(LENGTH_MEASURE(0.001),#10293,
'DISTANCE_ACCURACY_VALUE',
'Maximum model space distance between geometric entities at asserted c
onnectivities');
#10255=UNCERTAINTY_MEASURE_WITH_UNIT(LENGTH_MEASURE(0.001),#10293,
'DISTANCE_ACCURACY_VALUE',
'Maximum model space distance between geometric entities at asserted c
onnectivities');
#10256=UNCERTAINTY_MEASURE_WITH_UNIT(LENGTH_MEASURE(0.001),#10293,
'DISTANCE_ACCURACY_VALUE',
'Maximum model space distance between geometric entities at asserted c
onnectivities');
#10257=UNCERTAINTY_MEASURE_WITH_UNIT(LENGTH_MEASURE(0.001),#10293,
'DISTANCE_ACCURACY_VALUE',
'Maximum model space distance between geometric entities at asserted c
onnectivities');
#10258=UNCERTAINTY_MEASURE_WITH_UNIT(LENGTH_MEASURE(0.001),#10293,
'DISTANCE_ACCURACY_VALUE',
'Maximum model space distance between geometric entities at asserted c
onnectivities');
#10259=UNCERTAINTY_MEASURE_WITH_UNIT(LENGTH_MEASURE(0.001),#10293,
'DISTANCE_ACCURACY_VALUE',
'Maximum model space distance between geometric entities at asserted c
onnectivities');
#10260=UNCERTAINTY_MEASURE_WITH_UNIT(LENGTH_MEASURE(0.001),#10293,
'DISTANCE_ACCURACY_VALUE',
'Maximum model space distance between geometric entities at asserted c
onnectivities');
#10261=UNCERTAINTY_MEASURE_WITH_UNIT(LENGTH_MEASURE(0.001),#10293,
'DISTANCE_ACCURACY_VALUE',
'Maximum model space distance between geometric entities at asserted c
onnectivities');
#10262=UNCERTAINTY_MEASURE_WITH_UNIT(LENGTH_MEASURE(0.001),#10293,
'DISTANCE_ACCURACY_VALUE',
'Maximum model space distance between geometric entities at asserted c
onnectivities');
#10263=UNCERTAINTY_MEASURE_WITH_UNIT(LENGTH_MEASURE(0.001),#10293,
'DISTANCE_ACCURACY_VALUE',
'Maximum model space distance between geometric entities at asserted c
onnectivities');
#10264=UNCERTAINTY_MEASURE_WITH_UNIT(LENGTH_MEASURE(0.001),#10293,
'DISTANCE_ACCURACY_VALUE',
'Maximum model space distance between geometric entities at asserted c
onnectivities');
#10265=(
GEOMETRIC_REPRESENTATION_CONTEXT(3)
GLOBAL_UNCERTAINTY_ASSIGNED_CONTEXT((#10237))
GLOBAL_UNIT_ASSIGNED_CONTEXT((#10293,#10295,#10296))
REPRESENTATION_CONTEXT('','3D')
);
#10266=(
GEOMETRIC_REPRESENTATION_CONTEXT(3)
GLOBAL_UNCERTAINTY_ASSIGNED_CONTEXT((#10238))
GLOBAL_UNIT_ASSIGNED_CONTEXT((#10293,#10295,#10296))
REPRESENTATION_CONTEXT('','3D')
);
#10267=(
GEOMETRIC_REPRESENTATION_CONTEXT(3)
GLOBAL_UNCERTAINTY_ASSIGNED_CONTEXT((#10239))
GLOBAL_UNIT_ASSIGNED_CONTEXT((#10293,#10295,#10296))
REPRESENTATION_CONTEXT('','3D')
);
#10268=(
GEOMETRIC_REPRESENTATION_CONTEXT(3)
GLOBAL_UNCERTAINTY_ASSIGNED_CONTEXT((#10240))
GLOBAL_UNIT_ASSIGNED_CONTEXT((#10293,#10295,#10296))
REPRESENTATION_CONTEXT('','3D')
);
#10269=(
GEOMETRIC_REPRESENTATION_CONTEXT(3)
GLOBAL_UNCERTAINTY_ASSIGNED_CONTEXT((#10241))
GLOBAL_UNIT_ASSIGNED_CONTEXT((#10293,#10295,#10296))
REPRESENTATION_CONTEXT('','3D')
);
#10270=(
GEOMETRIC_REPRESENTATION_CONTEXT(3)
GLOBAL_UNCERTAINTY_ASSIGNED_CONTEXT((#10242))
GLOBAL_UNIT_ASSIGNED_CONTEXT((#10293,#10295,#10296))
REPRESENTATION_CONTEXT('','3D')
);
#10271=(
GEOMETRIC_REPRESENTATION_CONTEXT(3)
GLOBAL_UNCERTAINTY_ASSIGNED_CONTEXT((#10243))
GLOBAL_UNIT_ASSIGNED_CONTEXT((#10293,#10295,#10296))
REPRESENTATION_CONTEXT('','3D')
);
#10272=(
GEOMETRIC_REPRESENTATION_CONTEXT(3)
GLOBAL_UNCERTAINTY_ASSIGNED_CONTEXT((#10244))
GLOBAL_UNIT_ASSIGNED_CONTEXT((#10293,#10295,#10296))
REPRESENTATION_CONTEXT('','3D')
);
#10273=(
GEOMETRIC_REPRESENTATION_CONTEXT(3)
GLOBAL_UNCERTAINTY_ASSIGNED_CONTEXT((#10245))
GLOBAL_UNIT_ASSIGNED_CONTEXT((#10293,#10295,#10296))
REPRESENTATION_CONTEXT('','3D')
);
#10274=(
GEOMETRIC_REPRESENTATION_CONTEXT(3)
GLOBAL_UNCERTAINTY_ASSIGNED_CONTEXT((#10246))
GLOBAL_UNIT_ASSIGNED_CONTEXT((#10293,#10295,#10296))
REPRESENTATION_CONTEXT('','3D')
);
#10275=(
GEOMETRIC_REPRESENTATION_CONTEXT(3)
GLOBAL_UNCERTAINTY_ASSIGNED_CONTEXT((#10247))
GLOBAL_UNIT_ASSIGNED_CONTEXT((#10293,#10295,#10296))
REPRESENTATION_CONTEXT('','3D')
);
#10276=(
GEOMETRIC_REPRESENTATION_CONTEXT(3)
GLOBAL_UNCERTAINTY_ASSIGNED_CONTEXT((#10248))
GLOBAL_UNIT_ASSIGNED_CONTEXT((#10293,#10295,#10296))
REPRESENTATION_CONTEXT('','3D')
);
#10277=(
GEOMETRIC_REPRESENTATION_CONTEXT(3)
GLOBAL_UNCERTAINTY_ASSIGNED_CONTEXT((#10249))
GLOBAL_UNIT_ASSIGNED_CONTEXT((#10293,#10295,#10296))
REPRESENTATION_CONTEXT('','3D')
);
#10278=(
GEOMETRIC_REPRESENTATION_CONTEXT(3)
GLOBAL_UNCERTAINTY_ASSIGNED_CONTEXT((#10250))
GLOBAL_UNIT_ASSIGNED_CONTEXT((#10293,#10295,#10296))
REPRESENTATION_CONTEXT('','3D')
);
#10279=(
GEOMETRIC_REPRESENTATION_CONTEXT(3)
GLOBAL_UNCERTAINTY_ASSIGNED_CONTEXT((#10251))
GLOBAL_UNIT_ASSIGNED_CONTEXT((#10293,#10295,#10296))
REPRESENTATION_CONTEXT('','3D')
);
#10280=(
GEOMETRIC_REPRESENTATION_CONTEXT(3)
GLOBAL_UNCERTAINTY_ASSIGNED_CONTEXT((#10252))
GLOBAL_UNIT_ASSIGNED_CONTEXT((#10293,#10295,#10296))
REPRESENTATION_CONTEXT('','3D')
);
#10281=(
GEOMETRIC_REPRESENTATION_CONTEXT(3)
GLOBAL_UNCERTAINTY_ASSIGNED_CONTEXT((#10253))
GLOBAL_UNIT_ASSIGNED_CONTEXT((#10293,#10295,#10296))
REPRESENTATION_CONTEXT('','3D')
);
#10282=(
GEOMETRIC_REPRESENTATION_CONTEXT(3)
GLOBAL_UNCERTAINTY_ASSIGNED_CONTEXT((#10254))
GLOBAL_UNIT_ASSIGNED_CONTEXT((#10293,#10295,#10296))
REPRESENTATION_CONTEXT('','3D')
);
#10283=(
GEOMETRIC_REPRESENTATION_CONTEXT(3)
GLOBAL_UNCERTAINTY_ASSIGNED_CONTEXT((#10255))
GLOBAL_UNIT_ASSIGNED_CONTEXT((#10293,#10295,#10296))
REPRESENTATION_CONTEXT('','3D')
);
#10284=(
GEOMETRIC_REPRESENTATION_CONTEXT(3)
GLOBAL_UNCERTAINTY_ASSIGNED_CONTEXT((#10256))
GLOBAL_UNIT_ASSIGNED_CONTEXT((#10293,#10295,#10296))
REPRESENTATION_CONTEXT('','3D')
);
#10285=(
GEOMETRIC_REPRESENTATION_CONTEXT(3)
GLOBAL_UNCERTAINTY_ASSIGNED_CONTEXT((#10257))
GLOBAL_UNIT_ASSIGNED_CONTEXT((#10293,#10295,#10296))
REPRESENTATION_CONTEXT('','3D')
);
#10286=(
GEOMETRIC_REPRESENTATION_CONTEXT(3)
GLOBAL_UNCERTAINTY_ASSIGNED_CONTEXT((#10258))
GLOBAL_UNIT_ASSIGNED_CONTEXT((#10293,#10295,#10296))
REPRESENTATION_CONTEXT('','3D')
);
#10287=(
GEOMETRIC_REPRESENTATION_CONTEXT(3)
GLOBAL_UNCERTAINTY_ASSIGNED_CONTEXT((#10259))
GLOBAL_UNIT_ASSIGNED_CONTEXT((#10293,#10295,#10296))
REPRESENTATION_CONTEXT('','3D')
);
#10288=(
GEOMETRIC_REPRESENTATION_CONTEXT(3)
GLOBAL_UNCERTAINTY_ASSIGNED_CONTEXT((#10260))
GLOBAL_UNIT_ASSIGNED_CONTEXT((#10293,#10295,#10296))
REPRESENTATION_CONTEXT('','3D')
);
#10289=(
GEOMETRIC_REPRESENTATION_CONTEXT(3)
GLOBAL_UNCERTAINTY_ASSIGNED_CONTEXT((#10261))
GLOBAL_UNIT_ASSIGNED_CONTEXT((#10293,#10295,#10296))
REPRESENTATION_CONTEXT('','3D')
);
#10290=(
GEOMETRIC_REPRESENTATION_CONTEXT(3)
GLOBAL_UNCERTAINTY_ASSIGNED_CONTEXT((#10262))
GLOBAL_UNIT_ASSIGNED_CONTEXT((#10293,#10295,#10296))
REPRESENTATION_CONTEXT('','3D')
);
#10291=(
GEOMETRIC_REPRESENTATION_CONTEXT(3)
GLOBAL_UNCERTAINTY_ASSIGNED_CONTEXT((#10263))
GLOBAL_UNIT_ASSIGNED_CONTEXT((#10293,#10295,#10296))
REPRESENTATION_CONTEXT('','3D')
);
#10292=(
GEOMETRIC_REPRESENTATION_CONTEXT(3)
GLOBAL_UNCERTAINTY_ASSIGNED_CONTEXT((#10264))
GLOBAL_UNIT_ASSIGNED_CONTEXT((#10293,#10295,#10296))
REPRESENTATION_CONTEXT('','3D')
);
#10293=(
LENGTH_UNIT()
NAMED_UNIT(*)
SI_UNIT(.CENTI.,.METRE.)
);
#10294=(
LENGTH_UNIT()
NAMED_UNIT(*)
SI_UNIT($,.METRE.)
);
#10295=(
NAMED_UNIT(*)
PLANE_ANGLE_UNIT()
SI_UNIT($,.RADIAN.)
);
#10296=(
NAMED_UNIT(*)
SI_UNIT($,.STERADIAN.)
SOLID_ANGLE_UNIT()
);
#10297=SHAPE_DEFINITION_REPRESENTATION(#10324,#10413);
#10298=SHAPE_DEFINITION_REPRESENTATION(#10325,#10414);
#10299=SHAPE_DEFINITION_REPRESENTATION(#10326,#10415);
#10300=SHAPE_DEFINITION_REPRESENTATION(#10327,#10416);
#10301=SHAPE_DEFINITION_REPRESENTATION(#10328,#10417);
#10302=SHAPE_DEFINITION_REPRESENTATION(#10329,#10418);
#10303=SHAPE_DEFINITION_REPRESENTATION(#10330,#10419);
#10304=SHAPE_DEFINITION_REPRESENTATION(#10331,#10420);
#10305=SHAPE_DEFINITION_REPRESENTATION(#10332,#10421);
#10306=SHAPE_DEFINITION_REPRESENTATION(#10333,#10422);
#10307=SHAPE_DEFINITION_REPRESENTATION(#10334,#10423);
#10308=SHAPE_DEFINITION_REPRESENTATION(#10335,#10424);
#10309=SHAPE_DEFINITION_REPRESENTATION(#10336,#10425);
#10310=SHAPE_DEFINITION_REPRESENTATION(#10337,#10426);
#10311=SHAPE_DEFINITION_REPRESENTATION(#10338,#10427);
#10312=SHAPE_DEFINITION_REPRESENTATION(#10339,#10428);
#10313=SHAPE_DEFINITION_REPRESENTATION(#10340,#10429);
#10314=SHAPE_DEFINITION_REPRESENTATION(#10341,#10430);
#10315=SHAPE_DEFINITION_REPRESENTATION(#10342,#10431);
#10316=SHAPE_DEFINITION_REPRESENTATION(#10343,#10432);
#10317=SHAPE_DEFINITION_REPRESENTATION(#10344,#10433);
#10318=SHAPE_DEFINITION_REPRESENTATION(#10347,#10434);
#10319=SHAPE_DEFINITION_REPRESENTATION(#10348,#10435);
#10320=SHAPE_DEFINITION_REPRESENTATION(#10349,#10436);
#10321=SHAPE_DEFINITION_REPRESENTATION(#10387,#10437);
#10322=SHAPE_DEFINITION_REPRESENTATION(#10388,#10438);
#10323=SHAPE_DEFINITION_REPRESENTATION(#10389,#10439);
#10324=PRODUCT_DEFINITION_SHAPE('',$,#10441);
#10325=PRODUCT_DEFINITION_SHAPE('',$,#10442);
#10326=PRODUCT_DEFINITION_SHAPE('',$,#10443);
#10327=PRODUCT_DEFINITION_SHAPE('',$,#10444);
#10328=PRODUCT_DEFINITION_SHAPE('',$,#10445);
#10329=PRODUCT_DEFINITION_SHAPE('',$,#10446);
#10330=PRODUCT_DEFINITION_SHAPE('',$,#10447);
#10331=PRODUCT_DEFINITION_SHAPE('',$,#10448);
#10332=PRODUCT_DEFINITION_SHAPE('',$,#10449);
#10333=PRODUCT_DEFINITION_SHAPE('',$,#10450);
#10334=PRODUCT_DEFINITION_SHAPE('',$,#10451);
#10335=PRODUCT_DEFINITION_SHAPE('',$,#10452);
#10336=PRODUCT_DEFINITION_SHAPE('',$,#10453);
#10337=PRODUCT_DEFINITION_SHAPE('',$,#10454);
#10338=PRODUCT_DEFINITION_SHAPE('',$,#10455);
#10339=PRODUCT_DEFINITION_SHAPE('',$,#10456);
#10340=PRODUCT_DEFINITION_SHAPE('',$,#10457);
#10341=PRODUCT_DEFINITION_SHAPE('',$,#10458);
#10342=PRODUCT_DEFINITION_SHAPE('',$,#10459);
#10343=PRODUCT_DEFINITION_SHAPE('',$,#10460);
#10344=PRODUCT_DEFINITION_SHAPE('',$,#10461);
#10345=PRODUCT_DEFINITION_SHAPE($,$,#197);
#10346=PRODUCT_DEFINITION_SHAPE($,$,#198);
#10347=PRODUCT_DEFINITION_SHAPE('',$,#10462);
#10348=PRODUCT_DEFINITION_SHAPE('',$,#10463);
#10349=PRODUCT_DEFINITION_SHAPE('',$,#10464);
#10350=PRODUCT_DEFINITION_SHAPE($,$,#199);
#10351=PRODUCT_DEFINITION_SHAPE($,$,#200);
#10352=PRODUCT_DEFINITION_SHAPE($,$,#201);
#10353=PRODUCT_DEFINITION_SHAPE($,$,#202);
#10354=PRODUCT_DEFINITION_SHAPE($,$,#203);
#10355=PRODUCT_DEFINITION_SHAPE($,$,#204);
#10356=PRODUCT_DEFINITION_SHAPE($,$,#205);
#10357=PRODUCT_DEFINITION_SHAPE($,$,#206);
#10358=PRODUCT_DEFINITION_SHAPE($,$,#207);
#10359=PRODUCT_DEFINITION_SHAPE($,$,#208);
#10360=PRODUCT_DEFINITION_SHAPE($,$,#209);
#10361=PRODUCT_DEFINITION_SHAPE($,$,#210);
#10362=PRODUCT_DEFINITION_SHAPE($,$,#211);
#10363=PRODUCT_DEFINITION_SHAPE($,$,#212);
#10364=PRODUCT_DEFINITION_SHAPE($,$,#213);
#10365=PRODUCT_DEFINITION_SHAPE($,$,#214);
#10366=PRODUCT_DEFINITION_SHAPE($,$,#215);
#10367=PRODUCT_DEFINITION_SHAPE($,$,#216);
#10368=PRODUCT_DEFINITION_SHAPE($,$,#217);
#10369=PRODUCT_DEFINITION_SHAPE($,$,#218);
#10370=PRODUCT_DEFINITION_SHAPE($,$,#219);
#10371=PRODUCT_DEFINITION_SHAPE($,$,#220);
#10372=PRODUCT_DEFINITION_SHAPE($,$,#221);
#10373=PRODUCT_DEFINITION_SHAPE($,$,#222);
#10374=PRODUCT_DEFINITION_SHAPE($,$,#223);
#10375=PRODUCT_DEFINITION_SHAPE($,$,#224);
#10376=PRODUCT_DEFINITION_SHAPE($,$,#225);
#10377=PRODUCT_DEFINITION_SHAPE($,$,#226);
#10378=PRODUCT_DEFINITION_SHAPE($,$,#227);
#10379=PRODUCT_DEFINITION_SHAPE($,$,#228);
#10380=PRODUCT_DEFINITION_SHAPE($,$,#229);
#10381=PRODUCT_DEFINITION_SHAPE($,$,#230);
#10382=PRODUCT_DEFINITION_SHAPE($,$,#231);
#10383=PRODUCT_DEFINITION_SHAPE($,$,#232);
#10384=PRODUCT_DEFINITION_SHAPE($,$,#233);
#10385=PRODUCT_DEFINITION_SHAPE($,$,#234);
#10386=PRODUCT_DEFINITION_SHAPE($,$,#235);
#10387=PRODUCT_DEFINITION_SHAPE('',$,#10465);
#10388=PRODUCT_DEFINITION_SHAPE('',$,#10466);
#10389=PRODUCT_DEFINITION_SHAPE('',$,#10467);
#10390=PRODUCT_DEFINITION_SHAPE($,$,#236);
#10391=PRODUCT_DEFINITION_SHAPE($,$,#237);
#10392=PRODUCT_DEFINITION_SHAPE($,$,#238);
#10393=PRODUCT_DEFINITION_SHAPE($,$,#239);
#10394=PRODUCT_DEFINITION_SHAPE($,$,#240);
#10395=PRODUCT_DEFINITION_SHAPE($,$,#241);
#10396=PRODUCT_DEFINITION_SHAPE($,$,#242);
#10397=PRODUCT_DEFINITION_SHAPE($,$,#243);
#10398=PRODUCT_DEFINITION_SHAPE($,$,#244);
#10399=PRODUCT_DEFINITION_SHAPE($,$,#245);
#10400=PRODUCT_DEFINITION_SHAPE($,$,#246);
#10401=PRODUCT_DEFINITION_SHAPE($,$,#247);
#10402=PRODUCT_DEFINITION_SHAPE($,$,#248);
#10403=PRODUCT_DEFINITION_SHAPE($,$,#249);
#10404=PRODUCT_DEFINITION_SHAPE($,$,#250);
#10405=PRODUCT_DEFINITION_SHAPE($,$,#251);
#10406=PRODUCT_DEFINITION_SHAPE($,$,#252);
#10407=PRODUCT_DEFINITION_SHAPE($,$,#253);
#10408=PRODUCT_DEFINITION_SHAPE($,$,#254);
#10409=PRODUCT_DEFINITION_SHAPE($,$,#255);
#10410=PRODUCT_DEFINITION_SHAPE($,$,#256);
#10411=PRODUCT_DEFINITION_SHAPE($,$,#257);
#10412=PRODUCT_DEFINITION_SHAPE($,$,#258);
#10413=SHAPE_REPRESENTATION('',(#5289,#5862,#5863),#10265);
#10414=SHAPE_REPRESENTATION('',(#5290,#5760,#5761,#5762,#5763,#5764,#5765,
#5766,#5767,#5768,#5769,#5770,#5771,#5772,#5773,#5774,#5775,#5776,#5777,
#5778,#5779,#5780,#5781,#5782,#5783,#5784,#5785,#5786,#5787,#5788,#5789,
#5790,#5791,#5792,#5793,#5794,#5795,#5796),#10266);
#10415=SHAPE_REPRESENTATION('',(#5291),#10267);
#10416=SHAPE_REPRESENTATION('',(#5346),#10268);
#10417=SHAPE_REPRESENTATION('',(#5356),#10269);
#10418=SHAPE_REPRESENTATION('',(#5394),#10270);
#10419=SHAPE_REPRESENTATION('',(#5418),#10271);
#10420=SHAPE_REPRESENTATION('',(#5439),#10272);
#10421=SHAPE_REPRESENTATION('',(#5446),#10273);
#10422=SHAPE_REPRESENTATION('',(#5473),#10274);
#10423=SHAPE_REPRESENTATION('',(#5497),#10275);
#10424=SHAPE_REPRESENTATION('',(#5514),#10276);
#10425=SHAPE_REPRESENTATION('',(#5530),#10277);
#10426=SHAPE_REPRESENTATION('',(#5535),#10278);
#10427=SHAPE_REPRESENTATION('',(#5550),#10279);
#10428=SHAPE_REPRESENTATION('',(#5567,#5841,#5842,#5843,#5844,#5845,#5846,
#5847,#5848,#5849,#5850,#5851,#5852,#5853,#5854,#5855,#5856,#5857,#5858,
#5859,#5860,#5861),#10280);
#10429=SHAPE_REPRESENTATION('',(#5568),#10281);
#10430=SHAPE_REPRESENTATION('',(#5609),#10282);
#10431=SHAPE_REPRESENTATION('',(#5631,#5681,#5682),#10283);
#10432=SHAPE_REPRESENTATION('',(#5632),#10284);
#10433=SHAPE_REPRESENTATION('',(#5664),#10285);
#10434=SHAPE_REPRESENTATION('',(#5683),#10286);
#10435=SHAPE_REPRESENTATION('',(#5708),#10287);
#10436=SHAPE_REPRESENTATION('',(#5734),#10288);
#10437=SHAPE_REPRESENTATION('',(#5797),#10289);
#10438=SHAPE_REPRESENTATION('',(#5806),#10290);
#10439=SHAPE_REPRESENTATION('',(#5815),#10291);
#10440=PRODUCT_DEFINITION_CONTEXT('part definition',#10523,'design');
#10441=PRODUCT_DEFINITION('PAT-100','PAT-100',#10468,
#10440);
#10442=PRODUCT_DEFINITION('Shafts supports and end stops',
'Shafts supports and end stops',#10469,#10440);
#10443=PRODUCT_DEFINITION('Stop-mounted base plate',
'Stop-mounted base plate',#10470,#10440);
#10444=PRODUCT_DEFINITION('Precision Shaft - 12 mm Diameter, 300 mm Long',
'Precision Shaft - 12 mm Diameter, 300 mm Long',#10471,#10440);
#10445=PRODUCT_DEFINITION('Relieved shaft support',
'Relieved shaft support',#10472,#10440);
#10446=PRODUCT_DEFINITION('M5x14 Cap Screw','M5x14 Cap Screw',#10473,
#10440);
#10447=PRODUCT_DEFINITION('End stop','End stop',#10474,#10440);
#10448=PRODUCT_DEFINITION('Bonded stop pad','Bonded stop pad',#10475,
#10440);
#10449=PRODUCT_DEFINITION('Adjustable return-stop bracket',
'Adjustable return-stop bracket',#10476,#10440);
#10450=PRODUCT_DEFINITION('M5x14 Cap Screw (1)',
'M5x14 Cap Screw (1)',#10477,#10440);
#10451=PRODUCT_DEFINITION('Hex Bolt - M8x40','Hex Bolt - M8x40',
#10478,#10440);
#10452=PRODUCT_DEFINITION('Hex Nut - M8','Hex Nut - M8',#10479,
#10440);
#10453=PRODUCT_DEFINITION('Compression Spring - 2.5 mm Wire, 20 mm Outside Diameter, 60 mm Long',
'Compression Spring - 2.5 mm Wire, 20 mm Outside Diameter, 60 mm Long',
#10480,#10440);
#10454=PRODUCT_DEFINITION('Shaft collar','Shaft collar',#10481,
#10440);
#10455=PRODUCT_DEFINITION('Socket Set Screw - M5x8',
'Socket Set Screw - M5x8',#10482,#10440);
#10456=PRODUCT_DEFINITION('Two-bushing carriage',
'Two-bushing carriage',#10483,#10440);
#10457=PRODUCT_DEFINITION('Two-bushing housing',
'Two-bushing housing',#10484,#10440);
#10458=PRODUCT_DEFINITION('Carriage table','Carriage table',#10485,
#10440);
#10459=PRODUCT_DEFINITION('Linear Ball Bushing - 12 x 21 x 30 mm',
'Linear Ball Bushing - 12 x 21 x 30 mm',#10486,#10440);
#10460=PRODUCT_DEFINITION('Steel sleeve','Steel sleeve',#10487,
#10440);
#10461=PRODUCT_DEFINITION('Ball retainer (plastic)',
'Ball retainer (plastic)',#10488,#10440);
#10462=PRODUCT_DEFINITION('End retainer','End retainer',#10489,
#10440);
#10463=PRODUCT_DEFINITION('Cap Screw - M4x16','Cap Screw - M4x16',
#10490,#10440);
#10464=PRODUCT_DEFINITION('Cap Screw - M5x20','Cap Screw - M5x20',
#10491,#10440);
#10465=PRODUCT_DEFINITION('Grip','Grip',#10492,#10440);
#10466=PRODUCT_DEFINITION('Flat Washer - M6','Flat Washer - M6',
#10493,#10440);
#10467=PRODUCT_DEFINITION('Cap Screw - M6x25','Cap Screw - M6x25',
#10494,#10440);
#10468=PRODUCT_DEFINITION_FORMATION('',$,#10525);
#10469=PRODUCT_DEFINITION_FORMATION('',$,#10526);
#10470=PRODUCT_DEFINITION_FORMATION('',$,#10527);
#10471=PRODUCT_DEFINITION_FORMATION('',$,#10528);
#10472=PRODUCT_DEFINITION_FORMATION('',$,#10529);
#10473=PRODUCT_DEFINITION_FORMATION('',$,#10530);
#10474=PRODUCT_DEFINITION_FORMATION('',$,#10531);
#10475=PRODUCT_DEFINITION_FORMATION('',$,#10532);
#10476=PRODUCT_DEFINITION_FORMATION('',$,#10533);
#10477=PRODUCT_DEFINITION_FORMATION('',$,#10534);
#10478=PRODUCT_DEFINITION_FORMATION('',$,#10535);
#10479=PRODUCT_DEFINITION_FORMATION('',$,#10536);
#10480=PRODUCT_DEFINITION_FORMATION('',$,#10537);
#10481=PRODUCT_DEFINITION_FORMATION('',$,#10538);
#10482=PRODUCT_DEFINITION_FORMATION('',$,#10539);
#10483=PRODUCT_DEFINITION_FORMATION('',$,#10540);
#10484=PRODUCT_DEFINITION_FORMATION('',$,#10541);
#10485=PRODUCT_DEFINITION_FORMATION('',$,#10542);
#10486=PRODUCT_DEFINITION_FORMATION('',$,#10543);
#10487=PRODUCT_DEFINITION_FORMATION('',$,#10544);
#10488=PRODUCT_DEFINITION_FORMATION('',$,#10545);
#10489=PRODUCT_DEFINITION_FORMATION('',$,#10546);
#10490=PRODUCT_DEFINITION_FORMATION('',$,#10547);
#10491=PRODUCT_DEFINITION_FORMATION('',$,#10548);
#10492=PRODUCT_DEFINITION_FORMATION('',$,#10549);
#10493=PRODUCT_DEFINITION_FORMATION('',$,#10550);
#10494=PRODUCT_DEFINITION_FORMATION('',$,#10551);
#10495=PRODUCT_RELATED_PRODUCT_CATEGORY('PAT-100',
'PAT-100',(#10525));
#10496=PRODUCT_RELATED_PRODUCT_CATEGORY('Shafts supports and end stops',
'Shafts supports and end stops',(#10526));
#10497=PRODUCT_RELATED_PRODUCT_CATEGORY('Stop-mounted base plate',
'Stop-mounted base plate',(#10527));
#10498=PRODUCT_RELATED_PRODUCT_CATEGORY(
'Precision Shaft - 12 mm Diameter, 300 mm Long',
'Precision Shaft - 12 mm Diameter, 300 mm Long',(#10528));
#10499=PRODUCT_RELATED_PRODUCT_CATEGORY('Relieved shaft support',
'Relieved shaft support',(#10529));
#10500=PRODUCT_RELATED_PRODUCT_CATEGORY('M5x14 Cap Screw',
'M5x14 Cap Screw',(#10530));
#10501=PRODUCT_RELATED_PRODUCT_CATEGORY('End stop','End stop',(#10531));
#10502=PRODUCT_RELATED_PRODUCT_CATEGORY('Bonded stop pad',
'Bonded stop pad',(#10532));
#10503=PRODUCT_RELATED_PRODUCT_CATEGORY(
'Adjustable return-stop bracket','Adjustable return-stop bracket',(#10533));
#10504=PRODUCT_RELATED_PRODUCT_CATEGORY('M5x14 Cap Screw (1)',
'M5x14 Cap Screw (1)',(#10534));
#10505=PRODUCT_RELATED_PRODUCT_CATEGORY('Hex Bolt - M8x40',
'Hex Bolt - M8x40',(#10535));
#10506=PRODUCT_RELATED_PRODUCT_CATEGORY('Hex Nut - M8','Hex Nut - M8',(#10536));
#10507=PRODUCT_RELATED_PRODUCT_CATEGORY(
'Compression Spring - 2.5 mm Wire, 20 mm Outside Diameter, 60 mm Long',
'Compression Spring - 2.5 mm Wire, 20 mm Outside Diameter, 60 mm Long',
(#10537));
#10508=PRODUCT_RELATED_PRODUCT_CATEGORY('Shaft collar','Shaft collar',(#10538));
#10509=PRODUCT_RELATED_PRODUCT_CATEGORY('Socket Set Screw - M5x8',
'Socket Set Screw - M5x8',(#10539));
#10510=PRODUCT_RELATED_PRODUCT_CATEGORY('Two-bushing carriage',
'Two-bushing carriage',(#10540));
#10511=PRODUCT_RELATED_PRODUCT_CATEGORY('Two-bushing housing',
'Two-bushing housing',(#10541));
#10512=PRODUCT_RELATED_PRODUCT_CATEGORY('Carriage table',
'Carriage table',(#10542));
#10513=PRODUCT_RELATED_PRODUCT_CATEGORY(
'Linear Ball Bushing - 12 x 21 x 30 mm',
'Linear Ball Bushing - 12 x 21 x 30 mm',(#10543));
#10514=PRODUCT_RELATED_PRODUCT_CATEGORY('Steel sleeve','Steel sleeve',(#10544));
#10515=PRODUCT_RELATED_PRODUCT_CATEGORY('Ball retainer (plastic)',
'Ball retainer (plastic)',(#10545));
#10516=PRODUCT_RELATED_PRODUCT_CATEGORY('End retainer','End retainer',(#10546));
#10517=PRODUCT_RELATED_PRODUCT_CATEGORY('Cap Screw - M4x16',
'Cap Screw - M4x16',(#10547));
#10518=PRODUCT_RELATED_PRODUCT_CATEGORY('Cap Screw - M5x20',
'Cap Screw - M5x20',(#10548));
#10519=PRODUCT_RELATED_PRODUCT_CATEGORY('Grip','Grip',(#10549));
#10520=PRODUCT_RELATED_PRODUCT_CATEGORY('Flat Washer - M6',
'Flat Washer - M6',(#10550));
#10521=PRODUCT_RELATED_PRODUCT_CATEGORY('Cap Screw - M6x25',
'Cap Screw - M6x25',(#10551));
#10522=APPLICATION_PROTOCOL_DEFINITION('international standard',
'automotive_design',2009,#10523);
#10523=APPLICATION_CONTEXT(
'Core Data for Automotive Mechanical Design Process');
#10524=PRODUCT_CONTEXT('part definition',#10523,'mechanical');
#10525=PRODUCT('PAT-100','PAT-100','PAT-100',(#10524));
#10526=PRODUCT('Shafts supports and end stops',
'Shafts supports and end stops','Shafts supports and end stops',(#10524));
#10527=PRODUCT('Stop-mounted base plate','Stop-mounted base plate','Stop-mounted base plate',(#10524));
#10528=PRODUCT('Precision Shaft - 12 mm Diameter, 300 mm Long',
'Precision Shaft - 12 mm Diameter, 300 mm Long',
'Precision Shaft - 12 mm Diameter, 300 mm Long',(#10524));
#10529=PRODUCT('Relieved shaft support','Relieved shaft support',
'Relieved shaft support',(#10524));
#10530=PRODUCT('M5x14 Cap Screw','M5x14 Cap Screw',
'M5x14 Cap Screw',(#10524));
#10531=PRODUCT('End stop','End stop','End stop',(#10524));
#10532=PRODUCT('Bonded stop pad','Bonded stop pad',
'Bonded stop pad',(#10524));
#10533=PRODUCT('Adjustable return-stop bracket',
'Adjustable return-stop bracket','Adjustable return-stop bracket',(#10524));
#10534=PRODUCT('M5x14 Cap Screw (1)','M5x14 Cap Screw (1)',
'M5x14 Cap Screw (1)',(#10524));
#10535=PRODUCT('Hex Bolt - M8x40','Hex Bolt - M8x40',
'Hex Bolt - M8x40',(#10524));
#10536=PRODUCT('Hex Nut - M8','Hex Nut - M8','Hex Nut - M8',
(#10524));
#10537=PRODUCT('Compression Spring - 2.5 mm Wire, 20 mm Outside Diameter, 60 mm Long',
'Compression Spring - 2.5 mm Wire, 20 mm Outside Diameter, 60 mm Long',
'Compression Spring - 2.5 mm Wire, 20 mm Outside Diameter, 60 mm Long',
(#10524));
#10538=PRODUCT('Shaft collar','Shaft collar','Shaft collar',
(#10524));
#10539=PRODUCT('Socket Set Screw - M5x8','Socket Set Screw - M5x8',
'Socket Set Screw - M5x8',(#10524));
#10540=PRODUCT('Two-bushing carriage','Two-bushing carriage',
'Two-bushing carriage',(#10524));
#10541=PRODUCT('Two-bushing housing','Two-bushing housing',
'Two-bushing housing',(#10524));
#10542=PRODUCT('Carriage table','Carriage table',
'Carriage table',(#10524));
#10543=PRODUCT('Linear Ball Bushing - 12 x 21 x 30 mm',
'Linear Ball Bushing - 12 x 21 x 30 mm',
'Linear Ball Bushing - 12 x 21 x 30 mm',(#10524));
#10544=PRODUCT('Steel sleeve','Steel sleeve','Steel sleeve',
(#10524));
#10545=PRODUCT('Ball retainer (plastic)','Ball retainer (plastic)',
'Ball retainer (plastic)',(#10524));
#10546=PRODUCT('End retainer','End retainer','End retainer',
(#10524));
#10547=PRODUCT('Cap Screw - M4x16','Cap Screw - M4x16',
'Cap Screw - M4x16',(#10524));
#10548=PRODUCT('Cap Screw - M5x20','Cap Screw - M5x20',
'Cap Screw - M5x20',(#10524));
#10549=PRODUCT('Grip','Grip','Grip',(#10524));
#10550=PRODUCT('Flat Washer - M6','Flat Washer - M6',
'Flat Washer - M6',(#10524));
#10551=PRODUCT('Cap Screw - M6x25','Cap Screw - M6x25',
'Cap Screw - M6x25',(#10524));
#10552=PRESENTATION_STYLE_ASSIGNMENT((#10559));
#10553=PRESENTATION_STYLE_ASSIGNMENT((#10560));
#10554=PRESENTATION_STYLE_ASSIGNMENT((#10561));
#10555=PRESENTATION_STYLE_ASSIGNMENT((#10562));
#10556=PRESENTATION_STYLE_ASSIGNMENT((#10563));
#10557=PRESENTATION_STYLE_ASSIGNMENT((#10564));
#10558=PRESENTATION_STYLE_ASSIGNMENT((#10565));
#10559=SURFACE_STYLE_USAGE(.BOTH.,#10566);
#10560=SURFACE_STYLE_USAGE(.BOTH.,#10567);
#10561=SURFACE_STYLE_USAGE(.BOTH.,#10568);
#10562=SURFACE_STYLE_USAGE(.BOTH.,#10569);
#10563=SURFACE_STYLE_USAGE(.BOTH.,#10570);
#10564=SURFACE_STYLE_USAGE(.BOTH.,#10571);
#10565=SURFACE_STYLE_USAGE(.BOTH.,#10572);
#10566=SURFACE_SIDE_STYLE('',(#10573));
#10567=SURFACE_SIDE_STYLE('',(#10574));
#10568=SURFACE_SIDE_STYLE('',(#10575));
#10569=SURFACE_SIDE_STYLE('',(#10576));
#10570=SURFACE_SIDE_STYLE('',(#10577));
#10571=SURFACE_SIDE_STYLE('',(#10578));
#10572=SURFACE_SIDE_STYLE('',(#10579));
#10573=SURFACE_STYLE_FILL_AREA(#10580);
#10574=SURFACE_STYLE_FILL_AREA(#10581);
#10575=SURFACE_STYLE_FILL_AREA(#10582);
#10576=SURFACE_STYLE_FILL_AREA(#10583);
#10577=SURFACE_STYLE_FILL_AREA(#10584);
#10578=SURFACE_STYLE_FILL_AREA(#10585);
#10579=SURFACE_STYLE_FILL_AREA(#10586);
#10580=FILL_AREA_STYLE('Steel - Satin',(#10587));
#10581=FILL_AREA_STYLE('CAD Library Painted - Deep blue',(#10588));
#10582=FILL_AREA_STYLE('CAD Library Painted - Steel gray',(#10589));
#10583=FILL_AREA_STYLE('CAD Library Painted - Graphite',(#10590));
#10584=FILL_AREA_STYLE('CAD Library Painted - Engineering blue',(#10591));
#10585=FILL_AREA_STYLE('CAD Library Painted - Off white',(#10592));
#10586=FILL_AREA_STYLE('CAD Library Painted - Light blue',(#10593));
#10587=FILL_AREA_STYLE_COLOUR('Steel - Satin',#10594);
#10588=FILL_AREA_STYLE_COLOUR('CAD Library Painted - Deep blue',#10595);
#10589=FILL_AREA_STYLE_COLOUR('CAD Library Painted - Steel gray',#10596);
#10590=FILL_AREA_STYLE_COLOUR('CAD Library Painted - Graphite',#10597);
#10591=FILL_AREA_STYLE_COLOUR('CAD Library Painted - Engineering blue',
#10598);
#10592=FILL_AREA_STYLE_COLOUR('CAD Library Painted - Off white',#10599);
#10593=FILL_AREA_STYLE_COLOUR('CAD Library Painted - Light blue',#10600);
#10594=COLOUR_RGB('Steel - Satin',0.627450980392157,0.627450980392157,0.627450980392157);
#10595=COLOUR_RGB('CAD Library Painted - Deep blue',0.0784313725490196,
0.203921568627451,0.349019607843137);
#10596=COLOUR_RGB('CAD Library Painted - Steel gray',0.592156862745098,
0.631372549019608,0.67843137254902);
#10597=COLOUR_RGB('CAD Library Painted - Graphite',0.0980392156862745,0.109803921568627,
0.125490196078431);
#10598=COLOUR_RGB('CAD Library Painted - Engineering blue',0.12156862745098,
0.356862745098039,0.6);
#10599=COLOUR_RGB('CAD Library Painted - Off white',0.909803921568627,0.901960784313726,
0.858823529411765);
#10600=COLOUR_RGB('CAD Library Painted - Light blue',0.286274509803922,
0.552941176470588,0.780392156862745);
#10601=COLOUR_RGB('Dark Blue',0.08,0.2,0.34);
#10602=FILL_AREA_STYLE_COLOUR('',#10601);
#10603=FILL_AREA_STYLE('',(#10602));
#10604=SURFACE_STYLE_FILL_AREA(#10603);
#10605=SURFACE_SIDE_STYLE('',(#10604));
#10606=SURFACE_STYLE_USAGE(.BOTH.,#10605);
#10607=PRESENTATION_STYLE_ASSIGNMENT((#10606));
#10608=COLOUR_RGB('Light Blue',0.38,0.62,0.78);
#10609=FILL_AREA_STYLE_COLOUR('',#10608);
#10610=FILL_AREA_STYLE('',(#10609));
#10611=SURFACE_STYLE_FILL_AREA(#10610);
#10612=SURFACE_SIDE_STYLE('',(#10611));
#10613=SURFACE_STYLE_USAGE(.BOTH.,#10612);
#10614=PRESENTATION_STYLE_ASSIGNMENT((#10613));
#10615=COLOUR_RGB('Sky Blue',0.24,0.69,0.87);
#10616=FILL_AREA_STYLE_COLOUR('',#10615);
#10617=FILL_AREA_STYLE('',(#10616));
#10618=SURFACE_STYLE_FILL_AREA(#10617);
#10619=SURFACE_SIDE_STYLE('',(#10618));
#10620=SURFACE_STYLE_USAGE(.BOTH.,#10619);
#10621=PRESENTATION_STYLE_ASSIGNMENT((#10620));
#10622=COLOUR_RGB('Grey',0.48,0.52,0.57);
#10623=FILL_AREA_STYLE_COLOUR('',#10622);
#10624=FILL_AREA_STYLE('',(#10623));
#10625=SURFACE_STYLE_FILL_AREA(#10624);
#10626=SURFACE_SIDE_STYLE('',(#10625));
#10627=SURFACE_STYLE_USAGE(.BOTH.,#10626);
#10628=PRESENTATION_STYLE_ASSIGNMENT((#10627));
#10629=COLOUR_RGB('Black',0.12,0.14,0.17);
#10630=FILL_AREA_STYLE_COLOUR('',#10629);
#10631=FILL_AREA_STYLE('',(#10630));
#10632=SURFACE_STYLE_FILL_AREA(#10631);
#10633=SURFACE_SIDE_STYLE('',(#10632));
#10634=SURFACE_STYLE_USAGE(.BOTH.,#10633);
#10635=PRESENTATION_STYLE_ASSIGNMENT((#10634));
#10636=COLOUR_RGB('Off White',0.89,0.88,0.83);
#10637=FILL_AREA_STYLE_COLOUR('',#10636);
#10638=FILL_AREA_STYLE('',(#10637));
#10639=SURFACE_STYLE_FILL_AREA(#10638);
#10640=SURFACE_SIDE_STYLE('',(#10639));
#10641=SURFACE_STYLE_USAGE(.BOTH.,#10640);
#10642=PRESENTATION_STYLE_ASSIGNMENT((#10641));
ENDSEC;
END-ISO-10303-21;
